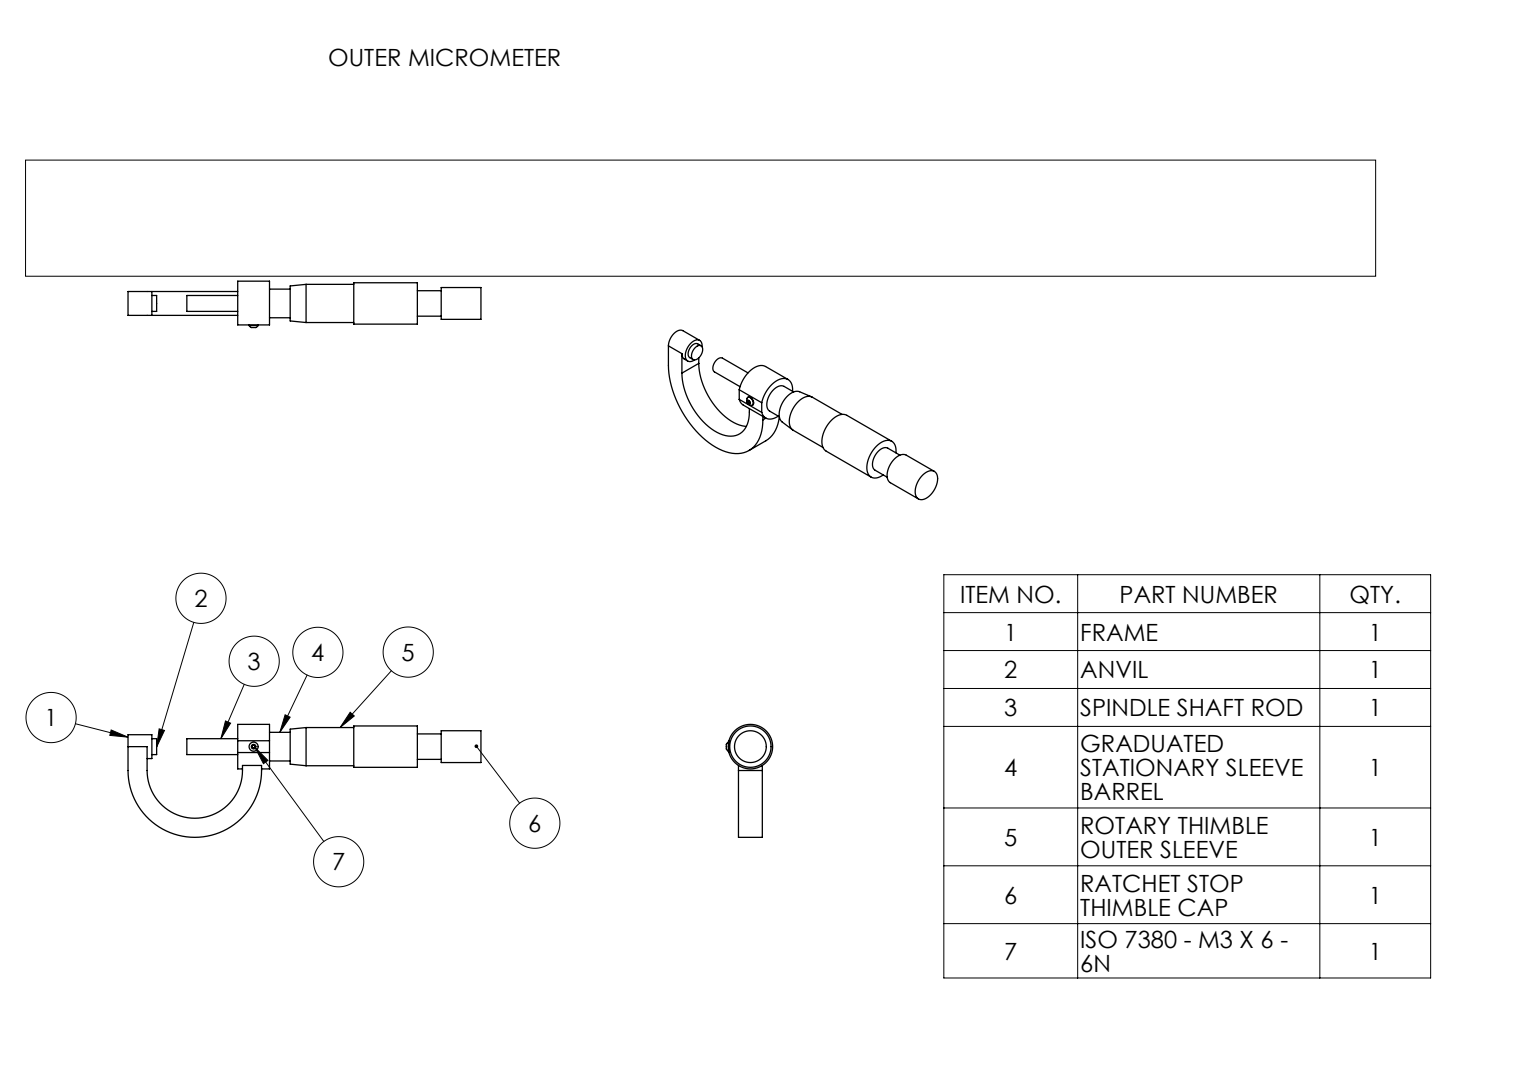
ISO-10303-21;
HEADER;
FILE_DESCRIPTION (('STEP AP214'),
    '1' );
FILE_NAME ('MAS-165',
    '2026-10-22T12:35:56',
    ( '' ),
    ( '' ),
    'SwSTEP 2.0',
    'SolidWorks 2026',
    '' );
FILE_SCHEMA (( 'AUTOMOTIVE_DESIGN' ));
ENDSEC;

DATA;
#1 = CARTESIAN_POINT ( 'NONE',  ( -30.00000000000000000, -8.316621552948000372E-15, 7.500000000000000000 ) ) ;
#2 = ORIENTED_EDGE ( 'NONE', *, *, #1476, .F. ) ;
#3 = EDGE_CURVE ( 'NONE', #403, #2721, #1745, .T. ) ;
#4 = DIRECTION ( 'NONE',  ( 0.000000000000000000, -1.000000000000000000, 0.000000000000000000 ) ) ;
#5 = FILL_AREA_STYLE_COLOUR ( '', #2827 ) ;
#6 = CYLINDRICAL_SURFACE ( 'NONE', #446, 5.000000000000000888 ) ;
#7 = EDGE_CURVE ( 'NONE', #417, #1789, #1947, .T. ) ;
#8 = PRODUCT_DEFINITION_SHAPE ( 'NONE', 'NONE',  #499 ) ;
#9 = PLANE ( 'NONE',  #1983 ) ;
#10 = VECTOR ( 'NONE', #970, 1000.000000000000000 ) ;
#11 = ORIENTED_EDGE ( 'NONE', *, *, #1483, .T. ) ;
#12 = VECTOR ( 'NONE', #2247, 1000.000000000000000 ) ;
#13 = ORIENTED_EDGE ( 'NONE', *, *, #713, .T. ) ;
#14 = VECTOR ( 'NONE', #2502, 1000.000000000000000 ) ;
#15 = CARTESIAN_POINT ( 'NONE',  ( 41.99999999999999289, -11.82159041753687845, 15.00000000000000000 ) ) ;
#16 = CARTESIAN_POINT ( 'NONE',  ( 37.48326775981565362, -1.423407605072588344, 16.38680797912482134 ) ) ;
#17 = DIRECTION ( 'NONE',  ( -0.000000000000000000, -0.000000000000000000, 1.000000000000000000 ) ) ;
#18 = STYLED_ITEM ( 'NONE', ( #223 ), #2456 ) ;
#19 = PRODUCT_DEFINITION_FORMATION_WITH_SPECIFIED_SOURCE ( 'ANY', '', #2257, .NOT_KNOWN. ) ;
#20 = LINE ( 'NONE', #2499, #1316 ) ;
#21 = PRESENTATION_STYLE_ASSIGNMENT (( #2824 ) ) ;
#22 = EDGE_LOOP ( 'NONE', ( #912, #3109, #1400, #258 ) ) ;
#23 = CARTESIAN_POINT ( 'NONE',  ( -26.99999999999999645, -7.622732162557277534E-15, 7.500000000000000000 ) ) ;
#24 = ADVANCED_FACE ( 'NONE', ( #42 ), #1841, .F. ) ;
#25 = DIRECTION ( 'NONE',  ( 0.000000000000000000, 0.000000000000000000, 1.000000000000000000 ) ) ;
#26 = CARTESIAN_POINT ( 'NONE',  ( 1.040000000000000036, 0.5773502691896263972, 1.000000000000000000 ) ) ;
#27 = MANIFOLD_SOLID_BREP ( 'Hex', #3139 ) ;
#28 = EDGE_CURVE ( 'NONE', #1232, #2394, #2025, .T. ) ;
#29 = ADVANCED_FACE ( 'NONE', ( #74 ), #315, .T. ) ;
#30 = ORIENTED_EDGE ( 'NONE', *, *, #3, .T. ) ;
#31 = CARTESIAN_POINT ( 'NONE',  ( 100.0000000000000000, -5.826660652933936785E-15, -1.499999999999999556 ) ) ;
#32 = CIRCLE ( 'NONE', #2124, 4.999999999999998224 ) ;
#33 = CARTESIAN_POINT ( 'NONE',  ( 30.00000000000000355, -15.00000000000000355, 15.00000000000000000 ) ) ;
#34 = DIRECTION ( 'NONE',  ( 1.000000000000000000, 2.312964634635742957E-16, 0.000000000000000000 ) ) ;
#35 = LINE ( 'NONE', #521, #2562 ) ;
#36 = CIRCLE ( 'NONE', #2432, 1.500000000000001332 ) ;
#37 = SHAPE_REPRESENTATION_RELATIONSHIP ( 'NONE' , 'NONE' ,  #2080, #2456 ) ;
#38 = EDGE_LOOP ( 'NONE', ( #1130, #2572 ) ) ;
#39 = DIRECTION ( 'NONE',  ( -0.000000000000000000, -0.000000000000000000, 1.000000000000000000 ) ) ;
#40 = DIRECTION ( 'NONE',  ( 0.000000000000000000, 0.000000000000000000, -1.000000000000000000 ) ) ;
#41 = CARTESIAN_POINT ( 'NONE',  ( 155.0000000000000284, -6.316519372592878167E-15, 2.499999999999999556 ) ) ;
#42 = FACE_OUTER_BOUND ( 'NONE', #272, .T. ) ;
#43 = ORIENTED_EDGE ( 'NONE', *, *, #1446, .F. ) ;
#44 = EDGE_CURVE ( 'NONE', #1232, #2037, #954, .T. ) ;
#45 = CIRCLE ( 'NONE', #370, 1.000000000000000000 ) ;
#46 = DIRECTION ( 'NONE',  ( 1.000000000000000000, 0.000000000000000000, 0.000000000000000000 ) ) ;
#47 = DIRECTION ( 'NONE',  ( 0.5150380749100542666, 1.049727191138618572E-16, 0.8571673007021122226 ) ) ;
#48 = DIRECTION ( 'NONE',  ( 0.000000000000000000, 1.000000000000000000, 0.000000000000000000 ) ) ;
#49 = ORIENTED_EDGE ( 'NONE', *, *, #85, .F. ) ;
#50 = SPHERICAL_SURFACE ( 'NONE', #2615, 3.351416843938785028 ) ;
#51 = EDGE_CURVE ( 'NONE', #357, #1877, #2331, .T. ) ;
#52 = ORIENTED_EDGE ( 'NONE', *, *, #1044, .F. ) ;
#53 = AXIS2_PLACEMENT_3D ( 'NONE', #2212, #1162, #2179 ) ;
#54 = CARTESIAN_POINT ( 'NONE',  ( 35.50000000000001421, 0.09798730130381244630, 16.49999999999999645 ) ) ;
#55 = DIRECTION ( 'NONE',  ( -0.000000000000000000, -0.000000000000000000, 1.000000000000000000 ) ) ;
#56 = VERTEX_POINT ( 'NONE', #623 ) ;
#57 = ORIENTED_EDGE ( 'NONE', *, *, #1286, .T. ) ;
#58 = VECTOR ( 'NONE', #2842, 1000.000000000000000 ) ;
#59 = DIRECTION ( 'NONE',  ( -1.000000000000000000, -0.000000000000000000, -0.000000000000000000 ) ) ;
#60 = DIRECTION ( 'NONE',  ( -2.478176394252581634E-16, 1.000000000000000000, 0.000000000000000000 ) ) ;
#61 = CLOSED_SHELL ( 'NONE', ( #1282, #587, #178, #1971, #3042, #967, #2402, #1991, #3073, #2520 ) ) ;
#62 = ADVANCED_FACE ( 'NONE', ( #2597 ), #606, .F. ) ;
#63 = COLOUR_RGB ( '',0.8941176470588234615, 0.8941176470588234615, 0.8941176470588234615 ) ;
#64 = ORIENTED_EDGE ( 'NONE', *, *, #1192, .F. ) ;
#65 = DIRECTION ( 'NONE',  ( 1.000000000000000000, 0.000000000000000000, 0.000000000000000000 ) ) ;
#66 = AXIS2_PLACEMENT_3D ( 'NONE', #1107, #1144, #2625 ) ;
#67 = CIRCLE ( 'NONE', #2220, 5.000000000000000000 ) ;
#68 = CARTESIAN_POINT ( 'NONE',  ( 180.0000000000000284, -6.928842772166554697E-15, 7.500000000000000000 ) ) ;
#69 = ORIENTED_EDGE ( 'NONE', *, *, #671, .F. ) ;
#70 = AXIS2_PLACEMENT_3D ( 'NONE', #1626, #2838, #1608 ) ;
#71 = CARTESIAN_POINT ( 'NONE',  ( 38.30162487582177278, 0.7519129166725618818, 16.46890859085320358 ) ) ;
#72 = DIRECTION ( 'NONE',  ( -0.000000000000000000, -0.000000000000000000, 1.000000000000000000 ) ) ;
#73 = CARTESIAN_POINT ( 'NONE',  ( 36.00776062886355078, -1.129166992945587866, 16.42915638304272363 ) ) ;
#74 = FACE_OUTER_BOUND ( 'NONE', #1738, .T. ) ;
#75 = ORIENTED_EDGE ( 'NONE', *, *, #1227, .F. ) ;
#76 = EDGE_CURVE ( 'NONE', #916, #1503, #2106, .T. ) ;
#77 = DIRECTION ( 'NONE',  ( 1.000000000000000000, 2.312964634635742957E-16, 0.000000000000000000 ) ) ;
#78 = CARTESIAN_POINT ( 'NONE',  ( 180.0000000000000284, -6.928842772166554697E-15, 7.500000000000000000 ) ) ;
#79 = VERTEX_POINT ( 'NONE', #2378 ) ;
#80 = DIRECTION ( 'NONE',  ( 1.000000000000000000, 0.000000000000000000, 0.000000000000000000 ) ) ;
#81 = AXIS2_PLACEMENT_3D ( 'NONE', #778, #1048, #1778 ) ;
#82 = CARTESIAN_POINT ( 'NONE',  ( 0.000000000000000000, -1.154700538379251684, -1.199226976249124676E-17 ) ) ;
#83 = ORIENTED_EDGE ( 'NONE', *, *, #909, .F. ) ;
#84 = AXIS2_PLACEMENT_3D ( 'NONE', #1775, #288, #1276 ) ;
#85 = EDGE_CURVE ( 'NONE', #373, #1694, #545, .T. ) ;
#86 = DIRECTION ( 'NONE',  ( -2.312964634635742957E-16, 1.000000000000000000, 0.000000000000000000 ) ) ;
#87 = VERTEX_POINT ( 'NONE', #874 ) ;
#88 = EDGE_LOOP ( 'NONE', ( #2505, #344, #500, #2889 ) ) ;
#89 = CARTESIAN_POINT ( 'NONE',  ( 70.00000000000032685, -6.928842772166554697E-15, 7.500000000000000000 ) ) ;
#90 = DIRECTION ( 'NONE',  ( -1.000000000000000000, -0.000000000000000000, -0.000000000000000000 ) ) ;
#91 = VERTEX_POINT ( 'NONE', #398 ) ;
#92 = CARTESIAN_POINT ( 'NONE',  ( 100.0000000000000000, -6.928842772166554697E-15, 7.500000000000000000 ) ) ;
#93 = CARTESIAN_POINT ( 'NONE',  ( 1.040000000000000036, 0.000000000000000000, 0.000000000000000000 ) ) ;
#94 = SHAPE_DEFINITION_REPRESENTATION ( #2508, #2591 ) ;
#95 = AXIS2_PLACEMENT_3D ( 'NONE', #1120, #2857, #636 ) ;
#96 = ORIENTED_EDGE ( 'NONE', *, *, #1476, .T. ) ;
#97 = ORIENTED_EDGE ( 'NONE', *, *, #671, .T. ) ;
#98 = DIRECTION ( 'NONE',  ( 0.000000000000000000, 0.000000000000000000, -1.000000000000000000 ) ) ;
#99 = CARTESIAN_POINT ( 'NONE',  ( 37.00000000000000000, 1.474514954580286030E-14, 20.99999999999999645 ) ) ;
#100 = ADVANCED_FACE ( 'NONE', ( #2884 ), #1598, .T. ) ;
#101 = EDGE_CURVE ( 'NONE', #738, #770, #2722, .T. ) ;
#102 = AXIS2_PLACEMENT_3D ( 'NONE', #2450, #1198, #3216 ) ;
#103 = PLANE ( 'NONE',  #1529 ) ;
#104 = EDGE_CURVE ( 'NONE', #415, #2077, #2930, .T. ) ;
#105 = ORIENTED_EDGE ( 'NONE', *, *, #2070, .F. ) ;
#106 = VERTEX_POINT ( 'NONE', #1616 ) ;
#107 = CARTESIAN_POINT ( 'NONE',  ( 38.45998082922275785, -0.3957415549423216605, 16.49311123862704775 ) ) ;
#108 = VERTEX_POINT ( 'NONE', #3091 ) ;
#109 =( REPRESENTATION_RELATIONSHIP ('NONE','NONE', #2426, #1116 ) REPRESENTATION_RELATIONSHIP_WITH_TRANSFORMATION ( #979 )SHAPE_REPRESENTATION_RELATIONSHIP( ) );
#110 = AXIS2_PLACEMENT_3D ( 'NONE', #2236, #2915, #685 ) ;
#111 = CARTESIAN_POINT ( 'NONE',  ( 0.000000000000000000, -0.5773502691896253980, -1.000000000000000000 ) ) ;
#112 = CLOSED_SHELL ( 'NONE', ( #233, #2010, #1720, #1045 ) ) ;
#113 = DIRECTION ( 'NONE',  ( 1.000000000000000000, 0.000000000000000000, 0.000000000000000000 ) ) ;
#114 = EDGE_LOOP ( 'NONE', ( #3092, #726, #1252, #1993 ) ) ;
#115 = CIRCLE ( 'NONE', #2264, 11.00000000000000355 ) ;
#116 = VECTOR ( 'NONE', #3173, 1000.000000000000000 ) ;
#117 = ORIENTED_EDGE ( 'NONE', *, *, #85, .T. ) ;
#118 = DIRECTION ( 'NONE',  ( 0.000000000000000000, 0.000000000000000000, -1.000000000000000000 ) ) ;
#119 = PRODUCT_DEFINITION_SHAPE ( 'NONE', 'NONE',  #694 ) ;
#120 = DIRECTION ( 'NONE',  ( 1.000000000000000000, 2.312964634635742957E-16, -0.000000000000000000 ) ) ;
#121 = AXIS2_PLACEMENT_3D ( 'NONE', #2014, #774, #60 ) ;
#122 = MECHANICAL_DESIGN_GEOMETRIC_PRESENTATION_REPRESENTATION (  '', ( #1113 ), #303 ) ;
#123 = ADVANCED_FACE ( 'NONE', ( #1123 ), #857, .F. ) ;
#124 = DIRECTION ( 'NONE',  ( 0.000000000000000000, 0.000000000000000000, 1.000000000000000000 ) ) ;
#125 = EDGE_LOOP ( 'NONE', ( #1383, #1724 ) ) ;
#126 = CARTESIAN_POINT ( 'NONE',  ( 38.49999999999999289, 1.474514954580286030E-14, 20.99999999999999645 ) ) ;
#127 = ADVANCED_FACE ( 'NONE', ( #378 ), #1155, .F. ) ;
#128 = ADVANCED_FACE ( 'NONE', ( #911 ), #1859, .T. ) ;
#129 = ORIENTED_EDGE ( 'NONE', *, *, #314, .F. ) ;
#130 = FACE_OUTER_BOUND ( 'NONE', #879, .T. ) ;
#131 = ORIENTED_EDGE ( 'NONE', *, *, #566, .F. ) ;
#132 = CARTESIAN_POINT ( 'NONE',  ( 155.0000000000000284, -5.949125332848671934E-15, -0.5000000000000004441 ) ) ;
#133 = APPLICATION_CONTEXT ( 'automotive_design' ) ;
#134 = CYLINDRICAL_SURFACE ( 'NONE', #2744, 14.00000000000000000 ) ;
#135 = DIRECTION ( 'NONE',  ( 0.000000000000000000, 0.000000000000000000, 1.000000000000000000 ) ) ;
#136 = ORIENTED_EDGE ( 'NONE', *, *, #525, .F. ) ;
#137 = VERTEX_POINT ( 'NONE', #2139 ) ;
#138 = DIRECTION ( 'NONE',  ( 0.000000000000000000, 0.000000000000000000, 1.000000000000000000 ) ) ;
#139 = DIRECTION ( 'NONE',  ( 0.000000000000000000, 0.000000000000000000, 1.000000000000000000 ) ) ;
#140 = CONICAL_SURFACE ( 'NONE', #2380, 1.250000000000001110, 1.029744258676654090 ) ;
#141 = DIRECTION ( 'NONE',  ( 0.000000000000000000, 0.5000000000000000000, -0.8660254037844385966 ) ) ;
#142 = ORIENTED_EDGE ( 'NONE', *, *, #1580, .F. ) ;
#143 = CARTESIAN_POINT ( 'NONE',  ( 38.49999999999997868, 0.1985404316418196702, 16.49999999999998224 ) ) ;
#144 = ORIENTED_EDGE ( 'NONE', *, *, #1772, .F. ) ;
#145 = CARTESIAN_POINT ( 'NONE',  ( 1.750000000000000000, 0.000000000000000000, 1.599999999999999645 ) ) ;
#146 = ORIENTED_EDGE ( 'NONE', *, *, #761, .F. ) ;
#147 = EDGE_CURVE ( 'NONE', #1882, #2430, #639, .T. ) ;
#148 = CYLINDRICAL_SURFACE ( 'NONE', #941, 7.500000000000000000 ) ;
#149 = PRODUCT_RELATED_PRODUCT_CATEGORY ( 'part', '', ( #2237 ) ) ;
#151 = EDGE_CURVE ( 'NONE', #2355, #2373, #2846, .T. ) ;
#150 = CARTESIAN_POINT ( 'NONE',  ( 140.0000000000000000, -6.928842772166554697E-15, 15.50000000000000000 ) ) ;
#152 = ORIENTED_EDGE ( 'NONE', *, *, #660, .F. ) ;
#153 = DIRECTION ( 'NONE',  ( -1.000000000000000000, -2.312964634635742957E-16, -0.000000000000000000 ) ) ;
#154 = CARTESIAN_POINT ( 'NONE',  ( 7.650000000000000355, 0.000000000000000000, 1.219500000000000028 ) ) ;
#155 = CIRCLE ( 'NONE', #2344, 1.219500000000000028 ) ;
#156 = SURFACE_STYLE_USAGE ( .BOTH. , #409 ) ;
#157 = CIRCLE ( 'NONE', #321, 1.000000000000000000 ) ;
#158 = CARTESIAN_POINT ( 'NONE',  ( 41.99999999999999289, 6.449497959004948951E-15, 15.00000000000000000 ) ) ;
#159 = ORIENTED_EDGE ( 'NONE', *, *, #497, .T. ) ;
#160 = DIRECTION ( 'NONE',  ( 0.000000000000000000, 0.000000000000000000, 1.000000000000000000 ) ) ;
#161 = AXIS2_PLACEMENT_3D ( 'NONE', #1164, #1184, #2943 ) ;
#162 = ORIENTED_EDGE ( 'NONE', *, *, #2964, .F. ) ;
#163 = VERTEX_POINT ( 'NONE', #411 ) ;
#164 = FACE_OUTER_BOUND ( 'NONE', #1049, .T. ) ;
#165 = ADVANCED_FACE ( 'NONE', ( #2345 ), #2393, .F. ) ;
#166 = CARTESIAN_POINT ( 'NONE',  ( 140.0000000000000000, -6.928842772166554697E-15, 7.500000000000000000 ) ) ;
#167 = DIRECTION ( 'NONE',  ( -0.000000000000000000, -0.000000000000000000, -1.000000000000000000 ) ) ;
#168 = PRODUCT_CONTEXT ( 'NONE', #3176, 'mechanical' ) ;
#169 = VERTEX_POINT ( 'NONE', #2407 ) ;
#170 = SURFACE_STYLE_USAGE ( .BOTH. , #3188 ) ;
#171 = FACE_OUTER_BOUND ( 'NONE', #213, .T. ) ;
#172 = AXIS2_PLACEMENT_3D ( 'NONE', #834, #880, #1605 ) ;
#173 = CIRCLE ( 'NONE', #1423, 12.00000000000000000 ) ;
#174 = CIRCLE ( 'NONE', #2003, 12.00000000000000000 ) ;
#175 = DIRECTION ( 'NONE',  ( 0.000000000000000000, -0.8660254037844387076, 0.5000000000000001110 ) ) ;
#176 = ADVANCED_FACE ( 'NONE', ( #427 ), #103, .T. ) ;
#177 = ORIENTED_EDGE ( 'NONE', *, *, #295, .F. ) ;
#178 = ADVANCED_FACE ( 'NONE', ( #1464 ), #509, .T. ) ;
#179 = DIRECTION ( 'NONE',  ( -2.312964634635742957E-16, 1.000000000000000000, 0.000000000000000000 ) ) ;
#180 = PRESENTATION_LAYER_ASSIGNMENT (  '', '', ( #18 ) ) ;
#181 = EDGE_LOOP ( 'NONE', ( #2444, #2735 ) ) ;
#182 = SURFACE_STYLE_FILL_AREA ( #1677 ) ;
#183 = ORIENTED_EDGE ( 'NONE', *, *, #207, .F. ) ;
#184 = EDGE_CURVE ( 'NONE', #3095, #2373, #706, .T. ) ;
#185 = DIRECTION ( 'NONE',  ( -0.000000000000000000, -0.000000000000000000, 1.000000000000000000 ) ) ;
#186 = CARTESIAN_POINT ( 'NONE',  ( 140.0000000000000000, -6.928842772166554697E-15, 12.50000000000000000 ) ) ;
#187 = CARTESIAN_POINT ( 'NONE',  ( -998.3826497308103853, 0.000000000000000000, 0.000000000000000000 ) ) ;
#188 = CONTEXT_DEPENDENT_SHAPE_REPRESENTATION ( #2861, #1874 ) ;
#189 =( LENGTH_UNIT ( ) NAMED_UNIT ( * ) SI_UNIT ( .MILLI., .METRE. ) );
#190 = DIRECTION ( 'NONE',  ( 1.000000000000000000, -0.000000000000000000, -0.000000000000000000 ) ) ;
#191 =( NAMED_UNIT ( * ) PLANE_ANGLE_UNIT ( ) SI_UNIT ( $, .RADIAN. ) );
#192 = EDGE_CURVE ( 'NONE', #1084, #211, #1163, .T. ) ;
#193 = CIRCLE ( 'NONE', #2951, 14.00000000000000000 ) ;
#194 = CARTESIAN_POINT ( 'NONE',  ( 155.0000000000000284, -6.928842772166554697E-15, 7.500000000000000000 ) ) ;
#195 = CIRCLE ( 'NONE', #1445, 10.00000000000000178 ) ;
#196 = CARTESIAN_POINT ( 'NONE',  ( 35.50000000000000000, 0.1959257125632855590, 16.50000000000000000 ) ) ;
#197 = ORIENTED_EDGE ( 'NONE', *, *, #540, .T. ) ;
#198 = CYLINDRICAL_SURFACE ( 'NONE', #340, 1.499999999999994449 ) ;
#199 = ORIENTED_EDGE ( 'NONE', *, *, #759, .F. ) ;
#200 = DIRECTION ( 'NONE',  ( 0.000000000000000000, 0.5000000000000003331, 0.8660254037844383745 ) ) ;
#201 = AXIS2_PLACEMENT_3D ( 'NONE', #1093, #2094, #1700 ) ;
#202 = DIRECTION ( 'NONE',  ( 1.000000000000000000, 0.000000000000000000, 0.000000000000000000 ) ) ;
#203 = DIRECTION ( 'NONE',  ( 0.000000000000000000, 1.224646799147353207E-16, -1.000000000000000000 ) ) ;
#204 = LINE ( 'NONE', #1443, #277 ) ;
#205 = SURFACE_STYLE_FILL_AREA ( #2455 ) ;
#206 = CONICAL_SURFACE ( 'NONE', #1038, 4.999999999999998224, 1.029744258676654312 ) ;
#207 = EDGE_CURVE ( 'NONE', #1415, #1866, #1103, .T. ) ;
#208 = DIRECTION ( 'NONE',  ( 0.000000000000000000, 0.000000000000000000, 1.000000000000000000 ) ) ;
#209 = DIRECTION ( 'NONE',  ( 1.000000000000000000, 0.000000000000000000, 0.000000000000000000 ) ) ;
#210 = ADVANCED_FACE ( 'NONE', ( #1707 ), #1221, .T. ) ;
#211 = VERTEX_POINT ( 'NONE', #3209 ) ;
#212 = CARTESIAN_POINT ( 'NONE',  ( 180.0000000000000284, -5.704195973019200848E-15, -2.500000000000002220 ) ) ;
#213 = EDGE_LOOP ( 'NONE', ( #2871, #2225, #753, #2533, #2320 ) ) ;
#214 = DIRECTION ( 'NONE',  ( -1.000000000000000000, -0.000000000000000000, -0.000000000000000000 ) ) ;
#215 = AXIS2_PLACEMENT_3D ( 'NONE', #2706, #2727, #977 ) ;
#216 = CARTESIAN_POINT ( 'NONE',  ( -41.99999999999999289, -6.449497959004950529E-15, 0.000000000000000000 ) ) ;
#217 = DIRECTION ( 'NONE',  ( 0.000000000000000000, 0.000000000000000000, -1.000000000000000000 ) ) ;
#218 = DIRECTION ( 'NONE',  ( 1.000000000000000000, 0.000000000000000000, 0.000000000000000000 ) ) ;
#219 = SURFACE_STYLE_FILL_AREA ( #3171 ) ;
#220 = EDGE_CURVE ( 'NONE', #2839, #2850, #1722, .T. ) ;
#221 = CYLINDRICAL_SURFACE ( 'NONE', #842, 2.849999999999999645 ) ;
#222 = PRODUCT_DEFINITION_SHAPE ( 'NONE', 'NONE',  #3226 ) ;
#223 = PRESENTATION_STYLE_ASSIGNMENT (( #983 ) ) ;
#224 = AXIS2_PLACEMENT_3D ( 'NONE', #361, #2327, #86 ) ;
#225 = PRESENTATION_LAYER_ASSIGNMENT (  '', '', ( #595 ) ) ;
#226 = AXIS2_PLACEMENT_3D ( 'NONE', #781, #362, #1550 ) ;
#227 = DIRECTION ( 'NONE',  ( -1.000000000000000000, -2.312964634635742957E-16, 0.000000000000000000 ) ) ;
#228 = DIRECTION ( 'NONE',  ( 1.000000000000000000, 0.000000000000000000, 0.000000000000000000 ) ) ;
#229 = AXIS2_PLACEMENT_3D ( 'NONE', #2936, #1181, #25 ) ;
#230 = CIRCLE ( 'NONE', #1844, 13.00000000000000178 ) ;
#231 = ORIENTED_EDGE ( 'NONE', *, *, #2924, .F. ) ;
#232 = EDGE_LOOP ( 'NONE', ( #1435, #2607, #784, #823 ) ) ;
#233 = ADVANCED_FACE ( 'NONE', ( #2687 ), #1203, .T. ) ;
#234 = EDGE_CURVE ( 'NONE', #516, #770, #260, .T. ) ;
#235 = CARTESIAN_POINT ( 'NONE',  ( 38.45202114561162432, -0.3888602178275583632, 16.49210820886665374 ) ) ;
#236 = CARTESIAN_POINT ( 'NONE',  ( 100.0000000000000000, -6.928842772166554697E-15, 19.50000000000000000 ) ) ;
#237 = CARTESIAN_POINT ( 'NONE',  ( 37.21237719682158485, -0.3527350612243344563, 12.48805154969246978 ) ) ;
#238 = LINE ( 'NONE', #2000, #1057 ) ;
#239 = CARTESIAN_POINT ( 'NONE',  ( 7.650000000000000355, 0.000000000000000000, 0.000000000000000000 ) ) ;
#240 =( NAMED_UNIT ( * ) PLANE_ANGLE_UNIT ( ) SI_UNIT ( $, .RADIAN. ) );
#241 = VERTEX_POINT ( 'NONE', #734 ) ;
#242 = CARTESIAN_POINT ( 'NONE',  ( -23.99999999999999645, 4.999999999999993783, 7.500000000000000888 ) ) ;
#243 = APPLICATION_CONTEXT ( 'automotive_design' ) ;
#244 = DIRECTION ( 'NONE',  ( 0.000000000000000000, 0.000000000000000000, 1.000000000000000000 ) ) ;
#245 = ORIENTED_EDGE ( 'NONE', *, *, #981, .F. ) ;
#246 = CIRCLE ( 'NONE', #2580, 14.00000000000000000 ) ;
#247 = ORIENTED_EDGE ( 'NONE', *, *, #3182, .F. ) ;
#248 = PRODUCT_DEFINITION_SHAPE ( 'NONE', 'NONE',  #1659 ) ;
#249 = DIRECTION ( 'NONE',  ( 0.000000000000000000, 0.000000000000000000, 1.000000000000000000 ) ) ;
#250 = DIRECTION ( 'NONE',  ( -1.000000000000000000, -0.000000000000000000, -0.000000000000000000 ) ) ;
#251 = DIRECTION ( 'NONE',  ( 0.000000000000000000, 0.000000000000000000, -1.000000000000000000 ) ) ;
#252 = EDGE_CURVE ( 'NONE', #466, #91, #1941, .T. ) ;
#253 = PRODUCT_CONTEXT ( 'NONE', #2801, 'mechanical' ) ;
#254 = PRODUCT_DEFINITION ( 'UNKNOWN', '', #1654, #571 ) ;
#255 = LINE ( 'NONE', #1808, #442 ) ;
#256 = CARTESIAN_POINT ( 'NONE',  ( -37.00000000000000000, -9.935696797193021379E-15, 7.500000000000000000 ) ) ;
#257 = EDGE_CURVE ( 'NONE', #3213, #626, #2525, .T. ) ;
#258 = ORIENTED_EDGE ( 'NONE', *, *, #2595, .F. ) ;
#259 = CARTESIAN_POINT ( 'NONE',  ( 27.00000000000000000, 6.704247063196759979E-15, 7.500000000000000000 ) ) ;
#260 = LINE ( 'NONE', #242, #2360 ) ;
#261 = LINE ( 'NONE', #26, #3174 ) ;
#262 = ORIENTED_EDGE ( 'NONE', *, *, #615, .T. ) ;
#263 = AXIS2_PLACEMENT_3D ( 'NONE', #1782, #798, #1552 ) ;
#264 = EDGE_LOOP ( 'NONE', ( #371, #711 ) ) ;
#265 = DIRECTION ( 'NONE',  ( 0.000000000000000000, 0.000000000000000000, 1.000000000000000000 ) ) ;
#266 = DIRECTION ( 'NONE',  ( -2.478176394252581634E-16, 1.000000000000000000, 0.000000000000000000 ) ) ;
#267 = CARTESIAN_POINT ( 'NONE',  ( 36.63069504892280293, -0.2100771151993728880, 12.49609970571322570 ) ) ;
#268 = AXIS2_PLACEMENT_3D ( 'NONE', #899, #2909, #681 ) ;
#269 = CYLINDRICAL_SURFACE ( 'NONE', #1531, 1.250000000000001110 ) ;
#270 = EDGE_CURVE ( 'NONE', #2818, #2355, #2189, .T. ) ;
#271 = DIRECTION ( 'NONE',  ( -1.000000000000000000, -0.000000000000000000, -0.000000000000000000 ) ) ;
#272 = EDGE_LOOP ( 'NONE', ( #2012, #2992, #144 ) ) ;
#273 = EDGE_CURVE ( 'NONE', #3128, #417, #1689, .T. ) ;
#274 = EDGE_CURVE ( 'NONE', #3069, #572, #2103, .T. ) ;
#275 = LINE ( 'NONE', #3009, #3087 ) ;
#276 = DIRECTION ( 'NONE',  ( 1.000000000000000000, 0.000000000000000000, 0.000000000000000000 ) ) ;
#277 = VECTOR ( 'NONE', #2201, 1000.000000000000000 ) ;
#278 = PRODUCT_DEFINITION_SHAPE ( 'NONE', 'NONE',  #3225 ) ;
#279 = CARTESIAN_POINT ( 'NONE',  ( -41.99999999999999289, -1.109217911451089172E-14, 0.000000000000000000 ) ) ;
#280 = AXIS2_PLACEMENT_3D ( 'NONE', #2473, #2667, #2948 ) ;
#281 = DIRECTION ( 'NONE',  ( 1.000000000000000000, 0.000000000000000000, -0.000000000000000000 ) ) ;
#282 = CIRCLE ( 'NONE', #2213, 4.999999999999999112 ) ;
#283 = ORIENTED_EDGE ( 'NONE', *, *, #1044, .T. ) ;
#284 = AXIS2_PLACEMENT_3D ( 'NONE', #1975, #461, #492 ) ;
#285 = VECTOR ( 'NONE', #856, 1000.000000000000000 ) ;
#286 = CARTESIAN_POINT ( 'NONE',  ( 140.0000000000000000, -6.316519372592878167E-15, 2.499999999999999556 ) ) ;
#287 = CARTESIAN_POINT ( 'NONE',  ( 38.19805860116020568, -0.9234461779904078460, 16.45357685834587613 ) ) ;
#288 = DIRECTION ( 'NONE',  ( 1.000000000000000000, 2.312964634635742957E-16, 0.000000000000000000 ) ) ;
#289 = LINE ( 'NONE', #2050, #12 ) ;
#290 = PRODUCT_DEFINITION_CONTEXT ( 'detailed design', #3029, 'design' ) ;
#291 = CARTESIAN_POINT ( 'NONE',  ( 1.040000000000000036, 0.8660254037844390407, 0.5000000000000002220 ) ) ;
#292 = FILL_AREA_STYLE_COLOUR ( '', #2366 ) ;
#293 = ORIENTED_EDGE ( 'NONE', *, *, #2633, .T. ) ;
#294 = DIRECTION ( 'NONE',  ( 1.000000000000000000, 0.000000000000000000, 0.000000000000000000 ) ) ;
#295 = EDGE_CURVE ( 'NONE', #1128, #2739, #2239, .T. ) ;
#296 = ADVANCED_FACE ( 'NONE', ( #1851 ), #6, .F. ) ;
#297 = PLANE ( 'NONE',  #1247 ) ;
#298 = EDGE_CURVE ( 'NONE', #3130, #2427, #2917, .T. ) ;
#299 = ORIENTED_EDGE ( 'NONE', *, *, #397, .F. ) ;
#300 = DIRECTION ( 'NONE',  ( 0.000000000000000000, 0.000000000000000000, -1.000000000000000000 ) ) ;
#301 = AXIS2_PLACEMENT_3D ( 'NONE', #323, #2823, #614 ) ;
#302 = FACE_OUTER_BOUND ( 'NONE', #2160, .T. ) ;
#303 =( GEOMETRIC_REPRESENTATION_CONTEXT ( 3 ) GLOBAL_UNCERTAINTY_ASSIGNED_CONTEXT ( ( #2916 ) ) GLOBAL_UNIT_ASSIGNED_CONTEXT ( ( #3088, #2138, #2843 ) ) REPRESENTATION_CONTEXT ( 'NONE', 'WORKASPACE' ) );
#304 = CARTESIAN_POINT ( 'NONE',  ( 180.0000000000000284, -6.928842772166554697E-15, 7.500000000000000000 ) ) ;
#305 = ORIENTED_EDGE ( 'NONE', *, *, #748, .T. ) ;
#306 = DIRECTION ( 'NONE',  ( -1.000000000000000000, -0.000000000000000000, -0.000000000000000000 ) ) ;
#307 = PRODUCT_DEFINITION_CONTEXT ( 'detailed design', #2566, 'design' ) ;
#308 = DIRECTION ( 'NONE',  ( -1.000000000000000000, -2.312964634635742957E-16, 0.000000000000000000 ) ) ;
#309 =( NAMED_UNIT ( * ) SI_UNIT ( $, .STERADIAN. ) SOLID_ANGLE_UNIT ( ) );
#310 = VERTEX_POINT ( 'NONE', #723 ) ;
#311 =( REPRESENTATION_RELATIONSHIP ('NONE','NONE', #2426, #524 ) REPRESENTATION_RELATIONSHIP_WITH_TRANSFORMATION ( #2435 )SHAPE_REPRESENTATION_RELATIONSHIP( ) );
#312 = CARTESIAN_POINT ( 'NONE',  ( 37.00000000000000000, 1.474514954580286030E-14, 20.99999999999999645 ) ) ;
#313 = FACE_OUTER_BOUND ( 'NONE', #2374, .T. ) ;
#314 = EDGE_CURVE ( 'NONE', #1882, #2739, #2737, .T. ) ;
#315 = SPHERICAL_SURFACE ( 'NONE', #1477, 3.351416843938785028 ) ;
#316 = ORIENTED_EDGE ( 'NONE', *, *, #1433, .F. ) ;
#317 = DIRECTION ( 'NONE',  ( -2.312964634635742957E-16, 1.000000000000000000, -0.000000000000000000 ) ) ;
#318 = DIRECTION ( 'NONE',  ( -1.000000000000000000, -0.000000000000000000, -0.000000000000000000 ) ) ;
#319 = CARTESIAN_POINT ( 'NONE',  ( 100.0000000000000000, -5.826660652933936785E-15, -1.499999999999999556 ) ) ;
#320 = ORIENTED_EDGE ( 'NONE', *, *, #1335, .T. ) ;
#321 = AXIS2_PLACEMENT_3D ( 'NONE', #2470, #438, #717 ) ;
#322 = DIRECTION ( 'NONE',  ( 0.000000000000000000, 0.000000000000000000, -1.000000000000000000 ) ) ;
#323 = CARTESIAN_POINT ( 'NONE',  ( 87.00000000000000000, -7.622732162557277534E-15, 7.500000000000000000 ) ) ;
#324 = ORIENTED_EDGE ( 'NONE', *, *, #2185, .F. ) ;
#325 = ADVANCED_FACE ( 'NONE', ( #447 ), #1432, .F. ) ;
#326 = VECTOR ( 'NONE', #1980, 1000.000000000000000 ) ;
#327 = CARTESIAN_POINT ( 'NONE',  ( 38.49999999999999289, 1.474514954580286030E-14, 16.49999999999999289 ) ) ;
#328 = CARTESIAN_POINT ( 'NONE',  ( 1.649999999999999911, 1.959434878635764737E-16, -1.599999999999999645 ) ) ;
#329 = EDGE_CURVE ( 'NONE', #2636, #2004, #2214, .T. ) ;
#330 = SHAPE_REPRESENTATION ( 'Spindle Shaft Rod', ( #2878 ), #1321 ) ;
#331 = CARTESIAN_POINT ( 'NONE',  ( 27.00000000000000000, -7.622732162557277534E-15, 7.500000000000000000 ) ) ;
#332 = ORIENTED_EDGE ( 'NONE', *, *, #28, .F. ) ;
#333 = CIRCLE ( 'NONE', #2770, 14.00000000000000000 ) ;
#334 = CARTESIAN_POINT ( 'NONE',  ( 1.040000000000000036, 0.5773502691896263972, 1.000000000000000000 ) ) ;
#335 = CARTESIAN_POINT ( 'NONE',  ( -30.00000000000000000, -3.673940397442059178E-15, 0.000000000000000000 ) ) ;
#336 = ORIENTED_EDGE ( 'NONE', *, *, #257, .F. ) ;
#337 = EDGE_CURVE ( 'NONE', #658, #1756, #1956, .T. ) ;
#338 = FACE_OUTER_BOUND ( 'NONE', #1623, .T. ) ;
#339 = AXIS2_PLACEMENT_3D ( 'NONE', #2130, #2093, #2543 ) ;
#340 = AXIS2_PLACEMENT_3D ( 'NONE', #664, #915, #276 ) ;
#341 = AXIS2_PLACEMENT_3D ( 'NONE', #259, #1766, #1051 ) ;
#342 = DIRECTION ( 'NONE',  ( -1.000000000000000000, -0.000000000000000000, -0.000000000000000000 ) ) ;
#343 = PRESENTATION_STYLE_ASSIGNMENT (( #1574 ) ) ;
#344 = ORIENTED_EDGE ( 'NONE', *, *, #354, .T. ) ;
#345 = DIRECTION ( 'NONE',  ( 1.000000000000000000, 0.000000000000000000, 0.000000000000000000 ) ) ;
#346 = CYLINDRICAL_SURFACE ( 'NONE', #226, 14.00000000000000000 ) ;
#347 = CARTESIAN_POINT ( 'NONE',  ( 180.0000000000000284, -6.928842772166554697E-15, 17.50000000000000000 ) ) ;
#348 =( LENGTH_UNIT ( ) NAMED_UNIT ( * ) SI_UNIT ( .MILLI., .METRE. ) );
#349 = ORIENTED_EDGE ( 'NONE', *, *, #2340, .F. ) ;
#350 = CARTESIAN_POINT ( 'NONE',  ( 1.040000000000000036, -0.5773502691896253980, -1.000000000000000000 ) ) ;
#351 = DIRECTION ( 'NONE',  ( -0.000000000000000000, -0.5000000000000003331, -0.8660254037844383745 ) ) ;
#352 = EDGE_LOOP ( 'NONE', ( #52, #897, #2546 ) ) ;
#353 = FACE_OUTER_BOUND ( 'NONE', #1646, .T. ) ;
#354 = EDGE_CURVE ( 'NONE', #2839, #488, #2984, .T. ) ;
#355 = FACE_OUTER_BOUND ( 'NONE', #984, .T. ) ;
#356 = DIRECTION ( 'NONE',  ( 1.000000000000000000, 0.000000000000000000, 0.000000000000000000 ) ) ;
#357 = VERTEX_POINT ( 'NONE', #15 ) ;
#358 = AXIS2_PLACEMENT_3D ( 'NONE', #894, #2425, #1157 ) ;
#359 = VERTEX_POINT ( 'NONE', #740 ) ;
#360 = ADVANCED_FACE ( 'NONE', ( #1740 ), #714, .F. ) ;
#361 = CARTESIAN_POINT ( 'NONE',  ( 47.00000000000000000, 1.133017633246824530E-14, 7.500000000000000000 ) ) ;
#362 = DIRECTION ( 'NONE',  ( 1.000000000000000000, 2.312964634635742957E-16, 0.000000000000000000 ) ) ;
#363 = DIRECTION ( 'NONE',  ( -0.000000000000000000, -0.000000000000000000, -1.000000000000000000 ) ) ;
#364 = ORIENTED_EDGE ( 'NONE', *, *, #2262, .F. ) ;
#365 = CARTESIAN_POINT ( 'NONE',  ( 35.65194399346783882, -0.6651260505907211629, 16.47584948644689007 ) ) ;
#366 = CARTESIAN_POINT ( 'NONE',  ( 38.50000000000000000, -0.1985404316418107051, 16.49999999999999645 ) ) ;
#367 = ORIENTED_EDGE ( 'NONE', *, *, #1335, .F. ) ;
#368 = CARTESIAN_POINT ( 'NONE',  ( 140.0000000000000000, -6.928842772166554697E-15, 7.500000000000000000 ) ) ;
#369 = DIRECTION ( 'NONE',  ( -0.000000000000000000, 1.000000000000000000, 1.224646799147353207E-16 ) ) ;
#370 = AXIS2_PLACEMENT_3D ( 'NONE', #3118, #1653, #1136 ) ;
#371 = ORIENTED_EDGE ( 'NONE', *, *, #1189, .F. ) ;
#372 = EDGE_CURVE ( 'NONE', #87, #2397, #1009, .T. ) ;
#373 = VERTEX_POINT ( 'NONE', #2492 ) ;
#374 = CARTESIAN_POINT ( 'NONE',  ( -23.99999999999999645, -6.928842772166554697E-15, 7.500000000000000000 ) ) ;
#375 = DIRECTION ( 'NONE',  ( -0.000000000000000000, -0.000000000000000000, 1.000000000000000000 ) ) ;
#376 = ADVANCED_FACE ( 'NONE', ( #502 ), #991, .T. ) ;
#377 = AXIS2_PLACEMENT_3D ( 'NONE', #2479, #250, #1805 ) ;
#378 = FACE_OUTER_BOUND ( 'NONE', #1451, .T. ) ;
#379 = ORIENTED_EDGE ( 'NONE', *, *, #1424, .F. ) ;
#380 = UNCERTAINTY_MEASURE_WITH_UNIT (LENGTH_MEASURE( 1.000000000000000082E-05 ), #1214, 'distance_accuracy_value', 'NONE');
#381 = FACE_BOUND ( 'NONE', #577, .T. ) ;
#382 = ORIENTED_EDGE ( 'NONE', *, *, #1088, .F. ) ;
#383 = FACE_OUTER_BOUND ( 'NONE', #1369, .T. ) ;
#384 = ORIENTED_EDGE ( 'NONE', *, *, #1446, .T. ) ;
#385 = CARTESIAN_POINT ( 'NONE',  ( 1.040000000000000036, 0.000000000000000000, 0.000000000000000000 ) ) ;
#386 = AXIS2_PLACEMENT_3D ( 'NONE', #1799, #2316, #40 ) ;
#387 = FACE_OUTER_BOUND ( 'NONE', #22, .T. ) ;
#388 = DIRECTION ( 'NONE',  ( 1.000000000000000000, 0.000000000000000000, 0.000000000000000000 ) ) ;
#389 = EDGE_LOOP ( 'NONE', ( #1124, #807, #247, #64 ) ) ;
#390 = AXIS2_PLACEMENT_3D ( 'NONE', #3020, #1047, #980 ) ;
#391 = VERTEX_POINT ( 'NONE', #2955 ) ;
#392 = VECTOR ( 'NONE', #317, 1000.000000000000000 ) ;
#393 = DIRECTION ( 'NONE',  ( -1.000000000000000000, -2.312964634635742957E-16, 0.000000000000000000 ) ) ;
#394 = DIRECTION ( 'NONE',  ( -0.000000000000000000, 0.5000000000000003331, -0.8660254037844383745 ) ) ;
#395 = AXIS2_PLACEMENT_3D ( 'NONE', #2044, #2788, #565 ) ;
#396 = MECHANICAL_DESIGN_GEOMETRIC_PRESENTATION_REPRESENTATION (  '', ( #2111 ), #1957 ) ;
#397 = EDGE_CURVE ( 'NONE', #1789, #2998, #1521, .T. ) ;
#398 = CARTESIAN_POINT ( 'NONE',  ( 155.0000000000000284, -6.928842772166554697E-15, 17.50000000000000000 ) ) ;
#399 = ORIENTED_EDGE ( 'NONE', *, *, #2047, .T. ) ;
#400 = DIRECTION ( 'NONE',  ( -1.000000000000000000, -0.000000000000000000, -0.000000000000000000 ) ) ;
#401 = VERTEX_POINT ( 'NONE', #1491 ) ;
#402 = CARTESIAN_POINT ( 'NONE',  ( 100.0000000000000000, -6.928842772166554697E-15, 20.50000000000000000 ) ) ;
#403 = VERTEX_POINT ( 'NONE', #1979 ) ;
#404 = CARTESIAN_POINT ( 'NONE',  ( 0.000000000000000000, 3.490243377569956061E-16, -2.849999999999999645 ) ) ;
#405 = CYLINDRICAL_SURFACE ( 'NONE', #2026, 12.00000000000000000 ) ;
#406 = ORIENTED_EDGE ( 'NONE', *, *, #733, .T. ) ;
#407 = DIRECTION ( 'NONE',  ( 0.000000000000000000, 0.000000000000000000, -1.000000000000000000 ) ) ;
#408 = DIRECTION ( 'NONE',  ( 1.000000000000000000, 0.000000000000000000, 0.000000000000000000 ) ) ;
#409 = SURFACE_SIDE_STYLE ('',( #2405 ) ) ;
#410 = VECTOR ( 'NONE', #420, 1000.000000000000000 ) ;
#411 = CARTESIAN_POINT ( 'NONE',  ( 27.00000000000000000, 1.243235845170086479E-14, 16.49999999999999289 ) ) ;
#412 = ORIENTED_EDGE ( 'NONE', *, *, #843, .T. ) ;
#413 = CARTESIAN_POINT ( 'NONE',  ( 100.0000000000000000, -6.928842772166554697E-15, 7.500000000000000000 ) ) ;
#414 = ADVANCED_FACE ( 'NONE', ( #2258 ), #2743, .F. ) ;
#415 = VERTEX_POINT ( 'NONE', #482 ) ;
#416 = CARTESIAN_POINT ( 'NONE',  ( 35.50000000000000000, -7.622732095468789599E-15, 16.49999999999999289 ) ) ;
#417 = VERTEX_POINT ( 'NONE', #1239 ) ;
#418 = PLANE ( 'NONE',  #2778 ) ;
#419 = UNCERTAINTY_MEASURE_WITH_UNIT (LENGTH_MEASURE( 1.000000000000000082E-05 ), #2203, 'distance_accuracy_value', 'NONE');
#420 = DIRECTION ( 'NONE',  ( 1.000000000000000000, 2.312964634635742957E-16, 0.000000000000000000 ) ) ;
#421 = ORIENTED_EDGE ( 'NONE', *, *, #1100, .F. ) ;
#422 = CARTESIAN_POINT ( 'NONE',  ( 38.49999999999999289, -7.622732162557277534E-15, 16.49999999999999289 ) ) ;
#423 = DIRECTION ( 'NONE',  ( -3.854941057726241055E-16, 1.000000000000000000, 0.000000000000000000 ) ) ;
#424 = VECTOR ( 'NONE', #2474, 1000.000000000000000 ) ;
#425 =( LENGTH_UNIT ( ) NAMED_UNIT ( * ) SI_UNIT ( .MILLI., .METRE. ) );
#426 = PRESENTATION_LAYER_ASSIGNMENT (  '', '', ( #2250 ) ) ;
#427 = FACE_OUTER_BOUND ( 'NONE', #2786, .T. ) ;
#428 = EDGE_LOOP ( 'NONE', ( #2332, #810, #725 ) ) ;
#429 = CARTESIAN_POINT ( 'NONE',  ( 37.09819064725438409, 1.500059831078516703, 16.37410956135321882 ) ) ;
#430 = ORIENTED_EDGE ( 'NONE', *, *, #981, .T. ) ;
#431 = FACE_OUTER_BOUND ( 'NONE', #2490, .T. ) ;
#432 = ORIENTED_EDGE ( 'NONE', *, *, #882, .F. ) ;
#433 = DIRECTION ( 'NONE',  ( 1.000000000000000000, 0.000000000000000000, 0.000000000000000000 ) ) ;
#434 = DIRECTION ( 'NONE',  ( -2.312964634635742957E-16, 1.000000000000000000, 0.000000000000000000 ) ) ;
#435 = DIRECTION ( 'NONE',  ( 1.000000000000000000, 2.312964634635742957E-16, 0.000000000000000000 ) ) ;
#436 = EDGE_CURVE ( 'NONE', #1803, #211, #2967, .T. ) ;
#437 = PRODUCT_CONTEXT ( 'NONE', #1344, 'mechanical' ) ;
#438 = DIRECTION ( 'NONE',  ( -1.000000000000000000, -0.000000000000000000, -0.000000000000000000 ) ) ;
#439 = VECTOR ( 'NONE', #888, 1000.000000000000227 ) ;
#440 = CARTESIAN_POINT ( 'NONE',  ( -41.99999999999999289, -15.00000000000000711, 15.00000000000000000 ) ) ;
#441 =( NAMED_UNIT ( * ) SI_UNIT ( $, .STERADIAN. ) SOLID_ANGLE_UNIT ( ) );
#442 = VECTOR ( 'NONE', #760, 1000.000000000000000 ) ;
#443 = CLOSED_SHELL ( 'NONE', ( #3157, #127, #2028, #1449, #2628, #1324, #3219, #537, #1757, #1948, #128, #2460, #2730, #325, #210, #2684, #2552, #1070, #2797, #829, #2086, #2736, #3198, #1675, #3211 ) ) ;
#444 = UNCERTAINTY_MEASURE_WITH_UNIT (LENGTH_MEASURE( 1.000000000000000082E-05 ), #3138, 'distance_accuracy_value', 'NONE');
#445 = AXIS2_PLACEMENT_3D ( 'NONE', #594, #3096, #3064 ) ;
#446 = AXIS2_PLACEMENT_3D ( 'NONE', #986, #1989, #749 ) ;
#447 = FACE_OUTER_BOUND ( 'NONE', #1253, .T. ) ;
#448 = CARTESIAN_POINT ( 'NONE',  ( 38.19805860116023410, 0.9234461779904211687, 16.45357685834586903 ) ) ;
#449 = EDGE_LOOP ( 'NONE', ( #2891, #1302, #2981, #2325 ) ) ;
#450 = CYLINDRICAL_SURFACE ( 'NONE', #386, 8.999999999999994671 ) ;
#451 = ORIENTED_EDGE ( 'NONE', *, *, #3048, .T. ) ;
#452 = CARTESIAN_POINT ( 'NONE',  ( -26.99999999999999645, -7.622732162557277534E-15, 7.500000000000000000 ) ) ;
#453 = CARTESIAN_POINT ( 'NONE',  ( 1.649999999999999911, 3.490243377569956061E-16, -2.849999999999999645 ) ) ;
#454 = DIRECTION ( 'NONE',  ( 0.000000000000000000, 0.000000000000000000, 1.000000000000000000 ) ) ;
#455 = FILL_AREA_STYLE_COLOUR ( '', #987 ) ;
#456 = EDGE_CURVE ( 'NONE', #1944, #79, #2985, .T. ) ;
#457 = DIRECTION ( 'NONE',  ( 0.000000000000000000, 0.000000000000000000, -1.000000000000000000 ) ) ;
#458 =( NAMED_UNIT ( * ) SI_UNIT ( $, .STERADIAN. ) SOLID_ANGLE_UNIT ( ) );
#459 =( REPRESENTATION_RELATIONSHIP ('NONE','NONE', #2426, #2080 ) REPRESENTATION_RELATIONSHIP_WITH_TRANSFORMATION ( #2729 )SHAPE_REPRESENTATION_RELATIONSHIP( ) );
#460 = VECTOR ( 'NONE', #601, 999.9999999999998863 ) ;
#461 = DIRECTION ( 'NONE',  ( -1.000000000000000000, -2.312964634635742957E-16, -0.000000000000000000 ) ) ;
#462 = AXIS2_PLACEMENT_3D ( 'NONE', #2599, #1915, #160 ) ;
#463 = DIRECTION ( 'NONE',  ( -0.000000000000000000, -0.000000000000000000, 1.000000000000000000 ) ) ;
#464 = ORIENTED_EDGE ( 'NONE', *, *, #1403, .T. ) ;
#465 = EDGE_CURVE ( 'NONE', #572, #3069, #67, .T. ) ;
#466 = VERTEX_POINT ( 'NONE', #347 ) ;
#467 = LINE ( 'NONE', #3149, #2202 ) ;
#468 = CARTESIAN_POINT ( 'NONE',  ( 38.12949724085409287, -0.9918543271721246279, 16.44544909559323287 ) ) ;
#469 = DIRECTION ( 'NONE',  ( -0.000000000000000000, -0.000000000000000000, -1.000000000000000000 ) ) ;
#470 = DIRECTION ( 'NONE',  ( 0.000000000000000000, 0.000000000000000000, -1.000000000000000000 ) ) ;
#471 = SURFACE_STYLE_FILL_AREA ( #953 ) ;
#472 = CARTESIAN_POINT ( 'NONE',  ( -5.000000000000000000, -6.316519372592878167E-15, 12.50000000000000000 ) ) ;
#473 = AXIS2_PLACEMENT_3D ( 'NONE', #1752, #228, #2224 ) ;
#474 = CARTESIAN_POINT ( 'NONE',  ( 1.040000000000000036, 0.5773502691896263972, -1.000000000000000000 ) ) ;
#475 = ADVANCED_FACE ( 'NONE', ( #1758, #2466 ), #1952, .F. ) ;
#476 = TOROIDAL_SURFACE ( 'NONE', #2813, 1.599999999999999645, 0.1000000000000000056 ) ;
#477 = LINE ( 'NONE', #1223, #1086 ) ;
#478 = EDGE_LOOP ( 'NONE', ( #2640, #2192 ) ) ;
#479 = VERTEX_POINT ( 'NONE', #286 ) ;
#480 = FACE_OUTER_BOUND ( 'NONE', #886, .T. ) ;
#481 = B_SPLINE_CURVE_WITH_KNOTS ( 'NONE', 3,
 ( #609, #3129, #1643, #1588, #2584, #1338, #1883, #2554, #896, #1864 ),
 .UNSPECIFIED., .F., .F.,
 ( 4, 2, 2, 2, 4 ),
 ( 0.0002158803543021033892, 0.0005338002860526318500, 0.0008517202178031603108, 0.001169640149553688880, 0.001487560081304217232 ),
 .UNSPECIFIED. ) ;
#482 = CARTESIAN_POINT ( 'NONE',  ( 60.00000000000000000, -6.928842772166554697E-15, 16.50000000000000000 ) ) ;
#483 = FACE_OUTER_BOUND ( 'NONE', #2112, .T. ) ;
#484 = DIRECTION ( 'NONE',  ( 1.000000000000000000, 0.000000000000000000, 0.000000000000000000 ) ) ;
#485 = PRODUCT_CONTEXT ( 'NONE', #2078, 'mechanical' ) ;
#486 = DIRECTION ( 'NONE',  ( -1.000000000000000000, 0.000000000000000000, -0.000000000000000000 ) ) ;
#487 = SHAPE_REPRESENTATION_RELATIONSHIP ( 'NONE' , 'NONE' ,  #330, #3045 ) ;
#488 = VERTEX_POINT ( 'NONE', #1274 ) ;
#489=STYLED_ITEM('',(#3271),#1054);
#490 = AXIS2_PLACEMENT_3D ( 'NONE', #3159, #891, #141 ) ;
#491 =( GEOMETRIC_REPRESENTATION_CONTEXT ( 3 ) GLOBAL_UNCERTAINTY_ASSIGNED_CONTEXT ( ( #2017 ) ) GLOBAL_UNIT_ASSIGNED_CONTEXT ( ( #605, #1315, #1563 ) ) REPRESENTATION_CONTEXT ( 'NONE', 'WORKASPACE' ) );
#492 = DIRECTION ( 'NONE',  ( 0.000000000000000000, -1.000000000000000000, 0.000000000000000000 ) ) ;
#493 = CIRCLE ( 'NONE', #3140, 12.00000000000000000 ) ;
#494 = FACE_OUTER_BOUND ( 'NONE', #181, .T. ) ;
#495 = CIRCLE ( 'NONE', #1644, 13.00000000000000178 ) ;
#496 = AXIS2_PLACEMENT_3D ( 'NONE', #1455, #2509, #249 ) ;
#497 = EDGE_CURVE ( 'NONE', #2088, #3100, #2946, .T. ) ;
#498 = ORIENTED_EDGE ( 'NONE', *, *, #1931, .T. ) ;
#499 = PRODUCT_DEFINITION ( 'UNKNOWN', '', #758, #2762 ) ;
#500 = ORIENTED_EDGE ( 'NONE', *, *, #591, .T. ) ;
#501 = MECHANICAL_DESIGN_GEOMETRIC_PRESENTATION_REPRESENTATION (  '', ( #18 ), #1537 ) ;
#502 = FACE_OUTER_BOUND ( 'NONE', #3012, .T. ) ;
#503 = CARTESIAN_POINT ( 'NONE',  ( 7.650000000000000355, 0.000000000000000000, 0.000000000000000000 ) ) ;
#504 = PLANE ( 'NONE',  #2021 ) ;
#505 = FACE_BOUND ( 'NONE', #645, .T. ) ;
#506 =( NAMED_UNIT ( * ) SI_UNIT ( $, .STERADIAN. ) SOLID_ANGLE_UNIT ( ) );
#507 = EDGE_LOOP ( 'NONE', ( #1692, #1273, #197, #3052 ) ) ;
#508 = CARTESIAN_POINT ( 'NONE',  ( 35.50982285435565444, 0.1975270956567308500, 16.49834805537327043 ) ) ;
#509 = CYLINDRICAL_SURFACE ( 'NONE', #747, 8.000000000000000000 ) ;
#510 = EDGE_CURVE ( 'NONE', #211, #1084, #174, .T. ) ;
#511 = DIRECTION ( 'NONE',  ( 1.000000000000000000, 0.000000000000000000, 0.000000000000000000 ) ) ;
#512 = CIRCLE ( 'NONE', #301, 8.999999999999992895 ) ;
#513 = ORIENTED_EDGE ( 'NONE', *, *, #2779, .F. ) ;
#514 = SHAPE_REPRESENTATION ( 'frame', ( #2878 ), #491 ) ;
#515 = CIRCLE ( 'NONE', #769, 14.00000000000000000 ) ;
#516 = VERTEX_POINT ( 'NONE', #608 ) ;
#517 = EDGE_CURVE ( 'NONE', #3213, #1108, #2029, .T. ) ;
#518 = CARTESIAN_POINT ( 'NONE',  ( 38.34772064623945198, -0.6658172387807467230, 16.47579882838004295 ) ) ;
#519 = DIRECTION ( 'NONE',  ( -0.000000000000000000, 0.5000000000000000000, 0.8660254037844385966 ) ) ;
#520 = CARTESIAN_POINT ( 'NONE',  ( 1.269999999999999796, 0.000000000000000000, 0.000000000000000000 ) ) ;
#521 = CARTESIAN_POINT ( 'NONE',  ( 1.040000000000000036, 1.154700538379252350, -1.084202172485497162E-16 ) ) ;
#522 = DIRECTION ( 'NONE',  ( -0.000000000000000000, -0.000000000000000000, 1.000000000000000000 ) ) ;
#523 = ORIENTED_EDGE ( 'NONE', *, *, #2382, .F. ) ;
#524 = SHAPE_REPRESENTATION ( 'socket button head screw_iso_ISO 7380 - M3 x 6 - 6N', ( #2878 ), #1010 ) ;
#525 = EDGE_CURVE ( 'NONE', #974, #2998, #2583, .T. ) ;
#526 = CARTESIAN_POINT ( 'NONE',  ( 37.92226537325436198, 1.198992358192679797, 16.42086068928975706 ) ) ;
#527 = SURFACE_STYLE_USAGE ( .BOTH. , #2428 ) ;
#528 = CARTESIAN_POINT ( 'NONE',  ( 100.0000000000000000, -5.459266613189731341E-15, -4.500000000000000888 ) ) ;
#529 = ORIENTED_EDGE ( 'NONE', *, *, #1753, .F. ) ;
#530 = CIRCLE ( 'NONE', #1202, 8.999999999999989342 ) ;
#531 = VERTEX_POINT ( 'NONE', #845 ) ;
#532 = DIRECTION ( 'NONE',  ( 1.000000000000000000, 2.312964634635742957E-16, 0.000000000000000000 ) ) ;
#533 = CARTESIAN_POINT ( 'NONE',  ( 37.99089481476345753, -1.130332597043731901, 16.42900728359812135 ) ) ;
#534 = PLANE ( 'NONE',  #3005 ) ;
#535 = VECTOR ( 'NONE', #185, 1000.000000000000000 ) ;
#536 = CYLINDRICAL_SURFACE ( 'NONE', #1581, 13.00000000000000178 ) ;
#537 = ADVANCED_FACE ( 'NONE', ( #579 ), #1568, .T. ) ;
#538 = CARTESIAN_POINT ( 'NONE',  ( -26.99999999999999645, -7.622732162557277534E-15, 7.500000000000000000 ) ) ;
#539 = ORIENTED_EDGE ( 'NONE', *, *, #274, .T. ) ;
#540 = EDGE_CURVE ( 'NONE', #2776, #241, #816, .T. ) ;
#541 = LINE ( 'NONE', #1281, #285 ) ;
#542 = SURFACE_STYLE_FILL_AREA ( #2023 ) ;
#543 = CIRCLE ( 'NONE', #2666, 9.000000000000000000 ) ;
#544 = CYLINDRICAL_SURFACE ( 'NONE', #1147, 5.000000000000000888 ) ;
#545 = CIRCLE ( 'NONE', #2775, 3.351416843938785028 ) ;
#546 = VERTEX_POINT ( 'NONE', #31 ) ;
#547 = CIRCLE ( 'NONE', #2359, 2.849999999999999645 ) ;
#548 = VERTEX_POINT ( 'NONE', #831 ) ;
#549 = VECTOR ( 'NONE', #1448, 1000.000000000000000 ) ;
#550 = CIRCLE ( 'NONE', #2314, 1.000000000000000000 ) ;
#551 = AXIS2_PLACEMENT_3D ( 'NONE', #3000, #773, #2215 ) ;
#552 = CARTESIAN_POINT ( 'NONE',  ( 35.80758137781342043, -0.9152444266664223615, 16.45371270176149991 ) ) ;
#553 = CARTESIAN_POINT ( 'NONE',  ( 35.68903409116789760, -0.7546922429561464529, 16.47012649564899078 ) ) ;
#554 = DIRECTION ( 'NONE',  ( -1.000000000000000000, -0.000000000000000000, -0.000000000000000000 ) ) ;
#555 = ORIENTED_EDGE ( 'NONE', *, *, #1912, .F. ) ;
#556 = CARTESIAN_POINT ( 'NONE',  ( 70.00000000000032685, -6.928842772166554697E-15, 19.50000000000000000 ) ) ;
#557 =( LENGTH_UNIT ( ) NAMED_UNIT ( * ) SI_UNIT ( .MILLI., .METRE. ) );
#558 = ORIENTED_EDGE ( 'NONE', *, *, #735, .T. ) ;
#559 = EDGE_CURVE ( 'NONE', #3128, #1393, #1428, .T. ) ;
#560 = PRODUCT_RELATED_PRODUCT_CATEGORY ( 'part', '', ( #2257 ) ) ;
#561 = CARTESIAN_POINT ( 'NONE',  ( 35.50000000000000000, 1.243235838461289750E-14, 16.49999999999999289 ) ) ;
#562 = CARTESIAN_POINT ( 'NONE',  ( 0.000000000000000000, -1.154700538379251684, -1.199226976249124676E-17 ) ) ;
#563 = DIRECTION ( 'NONE',  ( 0.000000000000000000, 0.000000000000000000, -1.000000000000000000 ) ) ;
#564 = ORIENTED_EDGE ( 'NONE', *, *, #1430, .T. ) ;
#565 = DIRECTION ( 'NONE',  ( 0.000000000000000000, 0.000000000000000000, 1.000000000000000000 ) ) ;
#566 = EDGE_CURVE ( 'NONE', #914, #391, #2569, .T. ) ;
#567 = DIRECTION ( 'NONE',  ( 0.000000000000000000, 0.000000000000000000, 1.000000000000000000 ) ) ;
#568 = FACE_OUTER_BOUND ( 'NONE', #2317, .T. ) ;
#569 = EDGE_LOOP ( 'NONE', ( #1118, #2896, #1520, #1946, #2140 ) ) ;
#570 = DIRECTION ( 'NONE',  ( 1.000000000000000000, 0.000000000000000000, 0.000000000000000000 ) ) ;
#571 = PRODUCT_DEFINITION_CONTEXT ( 'detailed design', #2741, 'design' ) ;
#572 = VERTEX_POINT ( 'NONE', #1304 ) ;
#573 = LINE ( 'NONE', #2313, #957 ) ;
#574 = DIRECTION ( 'NONE',  ( 1.000000000000000000, 0.000000000000000000, 0.000000000000000000 ) ) ;
#575 = EDGE_CURVE ( 'NONE', #2092, #576, #3015, .T. ) ;
#576 = VERTEX_POINT ( 'NONE', #1290 ) ;
#577 = EDGE_LOOP ( 'NONE', ( #3165, #2114 ) ) ;
#578 = CIRCLE ( 'NONE', #2085, 5.000000000000000888 ) ;
#579 = FACE_OUTER_BOUND ( 'NONE', #389, .T. ) ;
#580 = CARTESIAN_POINT ( 'NONE',  ( 1.040000000000000036, 0.5773502691896263972, 1.000000000000000000 ) ) ;
#581 = EDGE_LOOP ( 'NONE', ( #1628, #2886, #1194 ) ) ;
#582 = DIRECTION ( 'NONE',  ( 0.9950371902099894861, 1.218569110023196515E-17, 0.09950371902099541810 ) ) ;
#583 = CYLINDRICAL_SURFACE ( 'NONE', #2281, 10.00000000000000178 ) ;
#584 =( NAMED_UNIT ( * ) PLANE_ANGLE_UNIT ( ) SI_UNIT ( $, .RADIAN. ) );
#585 = VERTEX_POINT ( 'NONE', #1541 ) ;
#586 = CARTESIAN_POINT ( 'NONE',  ( -26.99999999999999645, -5.173438564262573782E-15, 12.49999999999999822 ) ) ;
#587 = ADVANCED_FACE ( 'NONE', ( #1804 ), #785, .F. ) ;
#588 = DIRECTION ( 'NONE',  ( 0.000000000000000000, 0.000000000000000000, -1.000000000000000000 ) ) ;
#589 = ORIENTED_EDGE ( 'NONE', *, *, #610, .T. ) ;
#590 = AXIS2_PLACEMENT_3D ( 'NONE', #2153, #2814, #139 ) ;
#591 = EDGE_CURVE ( 'NONE', #488, #815, #2290, .T. ) ;
#592 = AXIS2_PLACEMENT_3D ( 'NONE', #1852, #1310, #2370 ) ;
#593 = CARTESIAN_POINT ( 'NONE',  ( -30.00000000000000000, -3.673940397442059178E-15, 0.000000000000000000 ) ) ;
#594 = CARTESIAN_POINT ( 'NONE',  ( 7.369500000000001272, 0.000000000000000000, 0.000000000000000000 ) ) ;
#595=STYLED_ITEM('',(#3264),#27);
#596 = ORIENTED_EDGE ( 'NONE', *, *, #1551, .F. ) ;
#597 = CARTESIAN_POINT ( 'NONE',  ( 155.0000000000000284, -5.704195973019200848E-15, -2.500000000000002220 ) ) ;
#598 = EDGE_CURVE ( 'NONE', #1829, #1709, #1645, .T. ) ;
#599 = VECTOR ( 'NONE', #47, 1000.000000000000000 ) ;
#600 = AXIS2_PLACEMENT_3D ( 'NONE', #3063, #77, #3053 ) ;
#601 = DIRECTION ( 'NONE',  ( -0.7071067811865472397, 0.000000000000000000, 0.7071067811865479058 ) ) ;
#602 = ORIENTED_EDGE ( 'NONE', *, *, #1206, .T. ) ;
#603 =( GEOMETRIC_REPRESENTATION_CONTEXT ( 3 ) GLOBAL_UNCERTAINTY_ASSIGNED_CONTEXT ( ( #419 ) ) GLOBAL_UNIT_ASSIGNED_CONTEXT ( ( #2203, #1706, #998 ) ) REPRESENTATION_CONTEXT ( 'NONE', 'WORKASPACE' ) );
#604 = LINE ( 'NONE', #2391, #2518 ) ;
#605 =( LENGTH_UNIT ( ) NAMED_UNIT ( * ) SI_UNIT ( .MILLI., .METRE. ) );
#606 = PLANE ( 'NONE',  #1267 ) ;
#607 = ORIENTED_EDGE ( 'NONE', *, *, #667, .F. ) ;
#608 = CARTESIAN_POINT ( 'NONE',  ( -23.99999999999999645, 4.999999999999994671, 7.500000000000000888 ) ) ;
#609 = CARTESIAN_POINT ( 'NONE',  ( 36.58213974117523293, -6.323013916343274967E-15, 12.50000000000000178 ) ) ;
#610 = EDGE_CURVE ( 'NONE', #531, #1119, #1170, .T. ) ;
#611 = ORIENTED_EDGE ( 'NONE', *, *, #718, .T. ) ;
#612 = CARTESIAN_POINT ( 'NONE',  ( -26.99999999999999645, -5.785761963836251101E-15, 2.500000000000000444 ) ) ;
#613 = AXIS2_PLACEMENT_3D ( 'NONE', #951, #1199, #470 ) ;
#614 = DIRECTION ( 'NONE',  ( 0.000000000000000000, 1.000000000000000000, 0.000000000000000000 ) ) ;
#615 = EDGE_CURVE ( 'NONE', #1621, #241, #2725, .T. ) ;
#616 = DIRECTION ( 'NONE',  ( 1.000000000000000000, 0.000000000000000000, 0.000000000000000000 ) ) ;
#617 = ORIENTED_EDGE ( 'NONE', *, *, #252, .T. ) ;
#618 = CIRCLE ( 'NONE', #2483, 5.000000000000000000 ) ;
#619 = ORIENTED_EDGE ( 'NONE', *, *, #2326, .F. ) ;
#620 = FACE_OUTER_BOUND ( 'NONE', #1333, .T. ) ;
#621 = CARTESIAN_POINT ( 'NONE',  ( 36.58213974117523293, -6.323013916343274967E-15, 12.50000000000000178 ) ) ;
#622 = CIRCLE ( 'NONE', #2438, 1.219500000000000028 ) ;
#623 = CARTESIAN_POINT ( 'NONE',  ( -40.00430309513780003, -9.040569623688697978E-15, 7.500000000000000000 ) ) ;
#624 = EDGE_LOOP ( 'NONE', ( #2555, #789 ) ) ;
#625 = CARTESIAN_POINT ( 'NONE',  ( 37.38775466693719807, 1.452318184980633031, 16.38206869443958169 ) ) ;
#626 = VERTEX_POINT ( 'NONE', #1562 ) ;
#627 = CARTESIAN_POINT ( 'NONE',  ( 140.0000000000000000, -6.316519372592878167E-15, 2.499999999999999556 ) ) ;
#628 = VERTEX_POINT ( 'NONE', #2005 ) ;
#629 = DIRECTION ( 'NONE',  ( -2.312964634635742957E-16, 1.000000000000000000, 0.000000000000000000 ) ) ;
#630 = VECTOR ( 'NONE', #2703, 1000.000000000000000 ) ;
#631 = DIRECTION ( 'NONE',  ( -0.000000000000000000, -0.000000000000000000, -1.000000000000000000 ) ) ;
#632 = DIRECTION ( 'NONE',  ( 0.000000000000000000, 0.000000000000000000, 1.000000000000000000 ) ) ;
#633 =( GEOMETRIC_REPRESENTATION_CONTEXT ( 3 ) GLOBAL_UNCERTAINTY_ASSIGNED_CONTEXT ( ( #2364 ) ) GLOBAL_UNIT_ASSIGNED_CONTEXT ( ( #189, #684, #1683 ) ) REPRESENTATION_CONTEXT ( 'NONE', 'WORKASPACE' ) );
#634 = ORIENTED_EDGE ( 'NONE', *, *, #1634, .T. ) ;
#635 = ORIENTED_EDGE ( 'NONE', *, *, #2964, .T. ) ;
#636 = DIRECTION ( 'NONE',  ( 0.000000000000000000, 0.000000000000000000, -1.000000000000000000 ) ) ;
#637 = ADVANCED_FACE ( 'NONE', ( #2299 ), #812, .F. ) ;
#638 = LINE ( 'NONE', #3137, #2109 ) ;
#639 = LINE ( 'NONE', #1636, #1796 ) ;
#640 = VERTEX_POINT ( 'NONE', #1514 ) ;
#641 = DIRECTION ( 'NONE',  ( 1.000000000000000000, 0.000000000000000000, 0.000000000000000000 ) ) ;
#642 = APPLICATION_CONTEXT ( 'automotive_design' ) ;
#643 = ORIENTED_EDGE ( 'NONE', *, *, #44, .T. ) ;
#644 = DIRECTION ( 'NONE',  ( 0.000000000000000000, 0.000000000000000000, -1.000000000000000000 ) ) ;
#645 = EDGE_LOOP ( 'NONE', ( #2403, #3181 ) ) ;
#646 = PLANE ( 'NONE',  #339 ) ;
#647 = AXIS2_PLACEMENT_3D ( 'NONE', #686, #2975, #2223 ) ;
#648 = CARTESIAN_POINT ( 'NONE',  ( 7.650000000000000355, 0.000000000000000000, 1.219500000000000028 ) ) ;
#649 = CARTESIAN_POINT ( 'NONE',  ( 0.000000000000000000, 0.000000000000000000, 0.000000000000000000 ) ) ;
#650 = CIRCLE ( 'NONE', #1368, 8.999999999999994671 ) ;
#651 = ORIENTED_EDGE ( 'NONE', *, *, #2800, .T. ) ;
#652 = AXIS2_PLACEMENT_3D ( 'NONE', #1966, #1773, #964 ) ;
#653 = FACE_OUTER_BOUND ( 'NONE', #990, .T. ) ;
#654 = AXIS2_PLACEMENT_3D ( 'NONE', #452, #2165, #917 ) ;
#655 = CARTESIAN_POINT ( 'NONE',  ( 37.00000000000000000, 1.474514954580286030E-14, 12.99999999999999822 ) ) ;
#656 = SHAPE_REPRESENTATION_RELATIONSHIP ( 'NONE' , 'NONE' ,  #1116, #1362 ) ;
#657 = EDGE_CURVE ( 'NONE', #1365, #640, #2412, .T. ) ;
#658 = VERTEX_POINT ( 'NONE', #328 ) ;
#659 = DIRECTION ( 'NONE',  ( 0.000000000000000000, 0.000000000000000000, -1.000000000000000000 ) ) ;
#660 = EDGE_CURVE ( 'NONE', #1860, #1904, #1813, .T. ) ;
#661 = ORIENTED_EDGE ( 'NONE', *, *, #1385, .F. ) ;
#662 = DIRECTION ( 'NONE',  ( 1.000000000000000000, 2.312964634635742957E-16, 0.000000000000000000 ) ) ;
#663 = ORIENTED_EDGE ( 'NONE', *, *, #843, .F. ) ;
#664 = CARTESIAN_POINT ( 'NONE',  ( 37.00000000000000000, 1.474514954580286030E-14, 20.99999999999999645 ) ) ;
#665 = EDGE_LOOP ( 'NONE', ( #1180, #1453, #1135, #836 ) ) ;
#666 = CARTESIAN_POINT ( 'NONE',  ( 155.0000000000000284, -6.928842772166554697E-15, 7.500000000000000000 ) ) ;
#667 = EDGE_CURVE ( 'NONE', #531, #3100, #2993, .T. ) ;
#668 = LINE ( 'NONE', #730, #1764 ) ;
#669 = ORIENTED_EDGE ( 'NONE', *, *, #1688, .T. ) ;
#670 = SURFACE_STYLE_USAGE ( .BOTH. , #2897 ) ;
#671 = EDGE_CURVE ( 'NONE', #1489, #1964, #2710, .T. ) ;
#672 = CARTESIAN_POINT ( 'NONE',  ( 155.0000000000000284, -6.928842772166554697E-15, 7.500000000000000000 ) ) ;
#673 = VECTOR ( 'NONE', #1742, 1000.000000000000000 ) ;
#674 = CARTESIAN_POINT ( 'NONE',  ( 87.00000000000000000, -7.622732162557277534E-15, 7.500000000000000000 ) ) ;
#675 = ORIENTED_EDGE ( 'NONE', *, *, #1886, .F. ) ;
#676 = CARTESIAN_POINT ( 'NONE',  ( 35.68903409116789049, 0.7546922429561601087, 16.47012649564898368 ) ) ;
#677 = EDGE_CURVE ( 'NONE', #861, #1621, #573, .T. ) ;
#678 = ORIENTED_EDGE ( 'NONE', *, *, #3014, .F. ) ;
#679 = PLANE ( 'NONE',  #1059 ) ;
#680 = ORIENTED_EDGE ( 'NONE', *, *, #2129, .T. ) ;
#681 = DIRECTION ( 'NONE',  ( 0.000000000000000000, 1.000000000000000000, 0.000000000000000000 ) ) ;
#682 = CARTESIAN_POINT ( 'NONE',  ( 30.00000000000000355, -11.82159041753688200, 15.00000000000000000 ) ) ;
#683 = DIRECTION ( 'NONE',  ( 0.000000000000000000, 0.000000000000000000, 1.000000000000000000 ) ) ;
#684 =( NAMED_UNIT ( * ) PLANE_ANGLE_UNIT ( ) SI_UNIT ( $, .RADIAN. ) );
#685 = DIRECTION ( 'NONE',  ( 0.000000000000000000, 0.000000000000000000, 1.000000000000000000 ) ) ;
#686 = CARTESIAN_POINT ( 'NONE',  ( 3.469446951953614189E-15, -15.00000000000000355, 15.00000000000000000 ) ) ;
#687 = ORIENTED_EDGE ( 'NONE', *, *, #1176, .F. ) ;
#688 = AXIS2_PLACEMENT_3D ( 'NONE', #503, #2415, #965 ) ;
#689 = CARTESIAN_POINT ( 'NONE',  ( 35.50000000000000000, -7.622732095468789599E-15, 16.49999999999999289 ) ) ;
#690 = EDGE_LOOP ( 'NONE', ( #13, #3111, #3143, #1378, #349, #2589 ) ) ;
#691 = ORIENTED_EDGE ( 'NONE', *, *, #1656, .T. ) ;
#692 = EDGE_CURVE ( 'NONE', #3085, #1246, #230, .T. ) ;
#693 = CARTESIAN_POINT ( 'NONE',  ( -37.00000000000000000, -5.785761963836251101E-15, 2.500000000000001332 ) ) ;
#694 = PRODUCT_DEFINITION ( 'UNKNOWN', '', #708, #307 ) ;
#695 = CARTESIAN_POINT ( 'NONE',  ( -29.99999999999999645, -15.00000000000000355, 15.00000000000000000 ) ) ;
#696 = CARTESIAN_POINT ( 'NONE',  ( 87.00000000000000000, -7.010408762983600216E-15, 2.499999999999999556 ) ) ;
#697 = COLOUR_RGB ( '',0.8941176470588234615, 0.8941176470588234615, 0.8941176470588234615 ) ;
#698 = FACE_OUTER_BOUND ( 'NONE', #2603, .T. ) ;
#699 = CLOSED_SHELL ( 'NONE', ( #2287, #1331, #2040, #2558, #1386, #1530, #475, #2835, #165, #637, #795, #1234, #1613 ) ) ;
#700 = DIRECTION ( 'NONE',  ( 1.000000000000000000, 0.000000000000000000, 0.000000000000000000 ) ) ;
#701 = AXIS2_PLACEMENT_3D ( 'NONE', #3218, #2792, #1016 ) ;
#702 = VECTOR ( 'NONE', #227, 1000.000000000000000 ) ;
#703 = AXIS2_PLACEMENT_3D ( 'NONE', #1569, #2144, #2570 ) ;
#704 = VECTOR ( 'NONE', #1350, 1000.000000000000000 ) ;
#705 = COLOUR_RGB ( '',0.8941176470588234615, 0.8941176470588234615, 0.8941176470588234615 ) ;
#706 = LINE ( 'NONE', #474, #2158 ) ;
#707 = DIRECTION ( 'NONE',  ( -0.000000000000000000, -0.5000000000000000000, 0.8660254037844385966 ) ) ;
#708 = PRODUCT_DEFINITION_FORMATION_WITH_SPECIFIED_SOURCE ( 'ANY', '', #2285, .NOT_KNOWN. ) ;
#709 = ORIENTED_EDGE ( 'NONE', *, *, #2679, .T. ) ;
#710 = DIRECTION ( 'NONE',  ( 1.000000000000000000, -0.000000000000000000, -0.000000000000000000 ) ) ;
#711 = ORIENTED_EDGE ( 'NONE', *, *, #1812, .F. ) ;
#712 = DIRECTION ( 'NONE',  ( 1.000000000000000000, 0.000000000000000000, 0.000000000000000000 ) ) ;
#713 = EDGE_CURVE ( 'NONE', #1393, #3128, #2675, .T. ) ;
#714 = CYLINDRICAL_SURFACE ( 'NONE', #1903, 9.000000000000001776 ) ;
#715 = CARTESIAN_POINT ( 'NONE',  ( 140.0000000000000000, -6.316519372592878167E-15, 2.499999999999999556 ) ) ;
#716 = DIRECTION ( 'NONE',  ( 0.000000000000000000, 1.000000000000000000, 1.224646799147353207E-16 ) ) ;
#717 = DIRECTION ( 'NONE',  ( 0.000000000000000000, 0.000000000000000000, 1.000000000000000000 ) ) ;
#718 = EDGE_CURVE ( 'NONE', #310, #1076, #275, .T. ) ;
#719 = DIRECTION ( 'NONE',  ( -1.000000000000000000, 0.000000000000000000, -0.000000000000000000 ) ) ;
#720 = SURFACE_SIDE_STYLE ('',( #205 ) ) ;
#721 = EDGE_CURVE ( 'NONE', #1182, #169, #2268, .T. ) ;
#722 = AXIS2_PLACEMENT_3D ( 'NONE', #2605, #1834, #113 ) ;
#723 = CARTESIAN_POINT ( 'NONE',  ( 87.00000000000000000, -6.520550043324660412E-15, -1.499999999999992673 ) ) ;
#724 = CARTESIAN_POINT ( 'NONE',  ( 1.269999999999999796, -2.850000000000000533, -3.490243377569956061E-16 ) ) ;
#725 = ORIENTED_EDGE ( 'NONE', *, *, #2852, .F. ) ;
#726 = ORIENTED_EDGE ( 'NONE', *, *, #2442, .F. ) ;
#727 = DIRECTION ( 'NONE',  ( 0.000000000000000000, 1.000000000000000000, 0.000000000000000000 ) ) ;
#728 = CARTESIAN_POINT ( 'NONE',  ( 100.0000000000000000, -5.459266613189731341E-15, -4.500000000000000888 ) ) ;
#729 = FACE_OUTER_BOUND ( 'NONE', #989, .T. ) ;
#730 = CARTESIAN_POINT ( 'NONE',  ( 30.00000000000000355, -15.00000000000000355, 15.00000000000000000 ) ) ;
#731 = EDGE_CURVE ( 'NONE', #548, #738, #541, .T. ) ;
#732 = DIRECTION ( 'NONE',  ( 1.000000000000000000, 2.312964634635742957E-16, 0.000000000000000000 ) ) ;
#733 = EDGE_CURVE ( 'NONE', #2373, #626, #638, .T. ) ;
#734 = CARTESIAN_POINT ( 'NONE',  ( 38.25000000000000000, 1.474514954580286030E-14, 12.99999999999999822 ) ) ;
#735 = EDGE_CURVE ( 'NONE', #572, #1823, #604, .T. ) ;
#736 = CARTESIAN_POINT ( 'NONE',  ( 41.99999999999999289, -11.82159041753688022, 0.000000000000000000 ) ) ;
#737 = ORIENTED_EDGE ( 'NONE', *, *, #1525, .T. ) ;
#738 = VERTEX_POINT ( 'NONE', #1122 ) ;
#739 = AXIS2_PLACEMENT_3D ( 'NONE', #3054, #318, #567 ) ;
#740 = CARTESIAN_POINT ( 'NONE',  ( 140.0000000000000000, -6.928842772166554697E-15, 20.50000000000000000 ) ) ;
#741 = FACE_OUTER_BOUND ( 'NONE', #2868, .T. ) ;
#742 = CARTESIAN_POINT ( 'NONE',  ( 37.36887240208277916, -0.2104090322588208772, 12.49607929530250239 ) ) ;
#743 = CONTEXT_DEPENDENT_SHAPE_REPRESENTATION ( #2506, #222 ) ;
#744 = PLANE ( 'NONE',  #1838 ) ;
#745 = VERTEX_POINT ( 'NONE', #154 ) ;
#746 = VECTOR ( 'NONE', #732, 1000.000000000000000 ) ;
#747 = AXIS2_PLACEMENT_3D ( 'NONE', #194, #1501, #208 ) ;
#748 = EDGE_CURVE ( 'NONE', #79, #3095, #2563, .T. ) ;
#749 = DIRECTION ( 'NONE',  ( 0.000000000000000000, 0.000000000000000000, 1.000000000000000000 ) ) ;
#750 = DIRECTION ( 'NONE',  ( -0.000000000000000000, -0.000000000000000000, -1.000000000000000000 ) ) ;
#751 = AXIS2_PLACEMENT_3D ( 'NONE', #312, #39, #294 ) ;
#752 = ORIENTED_EDGE ( 'NONE', *, *, #2047, .F. ) ;
#753 = ORIENTED_EDGE ( 'NONE', *, *, #1619, .F. ) ;
#754 = AXIS2_PLACEMENT_3D ( 'NONE', #2606, #135, #388 ) ;
#755 = CARTESIAN_POINT ( 'NONE',  ( -5.000000000000000000, -6.928842772166554697E-15, 7.500000000000000000 ) ) ;
#756 = CARTESIAN_POINT ( 'NONE',  ( -37.00000000000000000, -5.173438564262574571E-15, 12.49999999999999645 ) ) ;
#757 = PLANE ( 'NONE',  #2282 ) ;
#758 = PRODUCT_DEFINITION_FORMATION_WITH_SPECIFIED_SOURCE ( 'ANY', '', #2237, .NOT_KNOWN. ) ;
#759 = EDGE_CURVE ( 'NONE', #626, #2346, #3103, .T. ) ;
#760 = DIRECTION ( 'NONE',  ( -1.000000000000000000, -0.000000000000000000, -0.000000000000000000 ) ) ;
#761 = EDGE_CURVE ( 'NONE', #3197, #2355, #2875, .T. ) ;
#762 = DIRECTION ( 'NONE',  ( 1.000000000000000000, 0.000000000000000000, 0.000000000000000000 ) ) ;
#763 = ORIENTED_EDGE ( 'NONE', *, *, #270, .F. ) ;
#764 = DIRECTION ( 'NONE',  ( 1.000000000000000000, 0.000000000000000000, 0.000000000000000000 ) ) ;
#765 = CARTESIAN_POINT ( 'NONE',  ( 1.649999999999999911, 0.000000000000000000, 0.000000000000000000 ) ) ;
#766 = DIRECTION ( 'NONE',  ( 1.000000000000000000, 0.000000000000000000, 0.000000000000000000 ) ) ;
#767 = AXIS2_PLACEMENT_3D ( 'NONE', #1954, #2911, #683 ) ;
#768 = ORIENTED_EDGE ( 'NONE', *, *, #610, .F. ) ;
#769 = AXIS2_PLACEMENT_3D ( 'NONE', #3204, #435, #2416 ) ;
#770 = VERTEX_POINT ( 'NONE', #1596 ) ;
#771 = ADVANCED_FACE ( 'NONE', ( #2358 ), #1893, .T. ) ;
#772 = EDGE_CURVE ( 'NONE', #1678, #1779, #333, .T. ) ;
#773 = DIRECTION ( 'NONE',  ( 1.000000000000000000, 2.312964634635742957E-16, 0.000000000000000000 ) ) ;
#774 = DIRECTION ( 'NONE',  ( 1.000000000000000000, 2.312964634635742957E-16, -0.000000000000000000 ) ) ;
#775 = DIRECTION ( 'NONE',  ( 1.000000000000000000, 0.000000000000000000, 0.000000000000000000 ) ) ;
#776 =( LENGTH_UNIT ( ) NAMED_UNIT ( * ) SI_UNIT ( .MILLI., .METRE. ) );
#777 = UNCERTAINTY_MEASURE_WITH_UNIT (LENGTH_MEASURE( 1.000000000000000082E-05 ), #1533, 'distance_accuracy_value', 'NONE');
#778 = CARTESIAN_POINT ( 'NONE',  ( -41.99999999999999289, -1.109217911451089172E-14, 7.500000000000000000 ) ) ;
#779 = VERTEX_POINT ( 'NONE', #586 ) ;
#780 = DIRECTION ( 'NONE',  ( -1.000000000000000000, -0.000000000000000000, -0.000000000000000000 ) ) ;
#781 = CARTESIAN_POINT ( 'NONE',  ( 27.00000000000000000, 6.704247063196759979E-15, 7.500000000000000000 ) ) ;
#782 = CARTESIAN_POINT ( 'NONE',  ( -26.99999999999999645, -5.785761963836251101E-15, 7.500000000000000000 ) ) ;
#783 = FILL_AREA_STYLE ('',( #1272 ) ) ;
#784 = ORIENTED_EDGE ( 'NONE', *, *, #2418, .T. ) ;
#785 = CYLINDRICAL_SURFACE ( 'NONE', #395, 5.000000000000000888 ) ;
#786 = DIRECTION ( 'NONE',  ( -0.7071067811865472397, 8.659560562354937789E-17, -0.7071067811865479058 ) ) ;
#787 = CARTESIAN_POINT ( 'NONE',  ( 37.41786025882473865, -0.1064896851603509553, 12.50000000000000178 ) ) ;
#788 = ADVANCED_FACE ( 'NONE', ( #1081 ), #2634, .T. ) ;
#789 = ORIENTED_EDGE ( 'NONE', *, *, #337, .T. ) ;
#790 = AXIS2_PLACEMENT_3D ( 'NONE', #2216, #1953, #2198 ) ;
#791 = CARTESIAN_POINT ( 'NONE',  ( 1.750000000000000000, 0.000000000000000000, 0.000000000000000000 ) ) ;
#792 = LINE ( 'NONE', #2780, #2329 ) ;
#793 =( NAMED_UNIT ( * ) SI_UNIT ( $, .STERADIAN. ) SOLID_ANGLE_UNIT ( ) );
#794 = ORIENTED_EDGE ( 'NONE', *, *, #28, .T. ) ;
#795 = ADVANCED_FACE ( 'NONE', ( #2578 ), #1099, .F. ) ;
#796 = CARTESIAN_POINT ( 'NONE',  ( 35.54829862735515889, 0.3901384415568778796, 16.49205630963118807 ) ) ;
#797 = CIRCLE ( 'NONE', #2874, 8.999999999999992895 ) ;
#798 = DIRECTION ( 'NONE',  ( 1.000000000000000000, 0.000000000000000000, 0.000000000000000000 ) ) ;
#799 = EDGE_CURVE ( 'NONE', #1823, #2935, #1473, .T. ) ;
#800 = CARTESIAN_POINT ( 'NONE',  ( 155.0000000000000284, -6.928842772166554697E-15, 12.50000000000000000 ) ) ;
#801 =( GEOMETRIC_REPRESENTATION_CONTEXT ( 3 ) GLOBAL_UNCERTAINTY_ASSIGNED_CONTEXT ( ( #1879 ) ) GLOBAL_UNIT_ASSIGNED_CONTEXT ( ( #776, #1509, #3040 ) ) REPRESENTATION_CONTEXT ( 'NONE', 'WORKASPACE' ) );
#802 = ORIENTED_EDGE ( 'NONE', *, *, #575, .T. ) ;
#803 = VECTOR ( 'NONE', #2318, 1000.000000000000227 ) ;
#804 = DIRECTION ( 'NONE',  ( 0.000000000000000000, -1.000000000000000000, 0.000000000000000000 ) ) ;
#805 = CARTESIAN_POINT ( 'NONE',  ( 35.75000000000000000, 1.489823039569627924E-14, 13.99999999999999822 ) ) ;
#806 = DIRECTION ( 'NONE',  ( 1.000000000000000000, 0.000000000000000000, 0.000000000000000000 ) ) ;
#807 = ORIENTED_EDGE ( 'NONE', *, *, #1490, .T. ) ;
#808 = APPLICATION_CONTEXT ( 'automotive_design' ) ;
#809 = COLOUR_RGB ( '',0.8941176470588234615, 0.8941176470588234615, 0.8941176470588234615 ) ;
#810 = ORIENTED_EDGE ( 'NONE', *, *, #517, .F. ) ;
#811 = EDGE_CURVE ( 'NONE', #546, #1226, #543, .T. ) ;
#812 = CYLINDRICAL_SURFACE ( 'NONE', #751, 1.499999999999994449 ) ;
#813 = CARTESIAN_POINT ( 'NONE',  ( 1.269999999999999796, 0.000000000000000000, 0.000000000000000000 ) ) ;
#814 = CARTESIAN_POINT ( 'NONE',  ( 1.040000000000000036, -1.154700538379251684, 0.000000000000000000 ) ) ;
#815 = VERTEX_POINT ( 'NONE', #872 ) ;
#816 = LINE ( 'NONE', #3033, #704 ) ;
#817 = AXIS2_PLACEMENT_3D ( 'NONE', #2148, #3132, #1968 ) ;
#818 = LINE ( 'NONE', #756, #599 ) ;
#819 = ORIENTED_EDGE ( 'NONE', *, *, #1576, .T. ) ;
#820 = DIRECTION ( 'NONE',  ( -0.000000000000000000, -0.5000000000000003331, -0.8660254037844383745 ) ) ;
#821 = DIRECTION ( 'NONE',  ( 0.000000000000000000, 0.000000000000000000, 1.000000000000000000 ) ) ;
#822 = SURFACE_STYLE_FILL_AREA ( #2068 ) ;
#823 = ORIENTED_EDGE ( 'NONE', *, *, #2248, .T. ) ;
#824 = ADVANCED_BREP_SHAPE_REPRESENTATION ( '', ( #27, #2878 ), #1010 ) ;
#825 = CARTESIAN_POINT ( 'NONE',  ( 35.80758137781341333, 0.9152444266664423456, 16.45371270176149991 ) ) ;
#826 = FILL_AREA_STYLE_COLOUR ( '', #63 ) ;
#827 = ADVANCED_FACE ( 'NONE', ( #1578 ), #3119, .T. ) ;
#828 = PRODUCT_RELATED_PRODUCT_CATEGORY ( 'part', '', ( #2771 ) ) ;
#829 = ADVANCED_FACE ( 'NONE', ( #1330, #2376 ), #1614, .T. ) ;
#830 = ORIENTED_EDGE ( 'NONE', *, *, #2211, .T. ) ;
#831 = CARTESIAN_POINT ( 'NONE',  ( -23.99999999999999645, -5.000000000000007994, 7.500000000000000000 ) ) ;
#832 = LINE ( 'NONE', #2833, #2937 ) ;
#833 = ORIENTED_EDGE ( 'NONE', *, *, #2536, .F. ) ;
#834 = CARTESIAN_POINT ( 'NONE',  ( 27.00000000000000000, 1.133017633246824530E-14, 7.500000000000000000 ) ) ;
#835 = DIRECTION ( 'NONE',  ( 1.000000000000000000, 2.312964634635742957E-16, 0.000000000000000000 ) ) ;
#836 = ORIENTED_EDGE ( 'NONE', *, *, #2343, .F. ) ;
#837 = DIRECTION ( 'NONE',  ( -0.000000000000000000, -0.000000000000000000, -1.000000000000000000 ) ) ;
#838 = LINE ( 'NONE', #2784, #2614 ) ;
#839 = EDGE_CURVE ( 'NONE', #1877, #916, #3032, .T. ) ;
#840 = ORIENTED_EDGE ( 'NONE', *, *, #1067, .T. ) ;
#841 = EDGE_LOOP ( 'NONE', ( #929, #2082, #634, #2585 ) ) ;
#842 = AXIS2_PLACEMENT_3D ( 'NONE', #2187, #3172, #938 ) ;
#843 = EDGE_CURVE ( 'NONE', #2350, #2807, #1836, .T. ) ;
#844 = VECTOR ( 'NONE', #820, 1000.000000000000114 ) ;
#845 = CARTESIAN_POINT ( 'NONE',  ( 35.50000000000000000, 1.492884656567496302E-14, 13.99999999999999822 ) ) ;
#846 = CARTESIAN_POINT ( 'NONE',  ( -29.99999999999999645, -15.00000000000000355, 15.00000000000000000 ) ) ;
#847 = ORIENTED_EDGE ( 'NONE', *, *, #1892, .F. ) ;
#848 = CARTESIAN_POINT ( 'NONE',  ( 0.000000000000000000, 0.5773502691896263972, -1.000000000000000000 ) ) ;
#849 = CIRCLE ( 'NONE', #2056, 9.000000000000000000 ) ;
#850 = AXIS2_PLACEMENT_3D ( 'NONE', #2539, #2547, #764 ) ;
#851 = FACE_OUTER_BOUND ( 'NONE', #1488, .T. ) ;
#852 = PRESENTATION_LAYER_ASSIGNMENT (  '', '', ( #2940 ) ) ;
#853 = DIRECTION ( 'NONE',  ( 0.000000000000000000, 0.000000000000000000, 1.000000000000000000 ) ) ;
#854 = EDGE_LOOP ( 'NONE', ( #691, #589 ) ) ;
#855 = ORIENTED_EDGE ( 'NONE', *, *, #1308, .T. ) ;
#856 = DIRECTION ( 'NONE',  ( -1.000000000000000000, -2.312964634635742957E-16, -0.000000000000000000 ) ) ;
#857 = PLANE ( 'NONE',  #1367 ) ;
#858 = EDGE_LOOP ( 'NONE', ( #30, #819 ) ) ;
#859 = ORIENTED_EDGE ( 'NONE', *, *, #1403, .F. ) ;
#860 = DIRECTION ( 'NONE',  ( 1.000000000000000000, 0.000000000000000000, 0.000000000000000000 ) ) ;
#861 = VERTEX_POINT ( 'NONE', #621 ) ;
#862 = ADVANCED_FACE ( 'NONE', ( #2594, #2858 ), #1684, .T. ) ;
#863 = CARTESIAN_POINT ( 'NONE',  ( 140.0000000000000000, -6.928842772166554697E-15, 12.50000000000000000 ) ) ;
#864 = CIRCLE ( 'NONE', #81, 7.500000000000000000 ) ;
#866 = EDGE_CURVE ( 'NONE', #106, #137, #2406, .T. ) ;
#865 = DIRECTION ( 'NONE',  ( 0.000000000000000000, 0.000000000000000000, 1.000000000000000000 ) ) ;
#867 = DIRECTION ( 'NONE',  ( 1.000000000000000000, 0.000000000000000000, 0.000000000000000000 ) ) ;
#868 = ORIENTED_EDGE ( 'NONE', *, *, #2571, .F. ) ;
#869 = VECTOR ( 'NONE', #662, 1000.000000000000000 ) ;
#870 = ORIENTED_EDGE ( 'NONE', *, *, #1061, .T. ) ;
#871 = FACE_OUTER_BOUND ( 'NONE', #3146, .T. ) ;
#872 = CARTESIAN_POINT ( 'NONE',  ( 1.750000000000000000, 0.000000000000000000, 1.499999999999999556 ) ) ;
#873 = UNCERTAINTY_MEASURE_WITH_UNIT (LENGTH_MEASURE( 1.000000000000000082E-05 ), #3007, 'distance_accuracy_value', 'NONE');
#874 = CARTESIAN_POINT ( 'NONE',  ( 47.00000000000000000, -13.99999999999998757, 7.500000000000001776 ) ) ;
#875 = EDGE_LOOP ( 'NONE', ( #768, #1279, #2791, #1807 ) ) ;
#876 = CARTESIAN_POINT ( 'NONE',  ( 38.49999999999999289, -7.622732162557277534E-15, 16.49999999999999289 ) ) ;
#877 = VERTEX_POINT ( 'NONE', #2663 ) ;
#878 = CARTESIAN_POINT ( 'NONE',  ( 155.0000000000000284, -6.928842772166554697E-15, 7.500000000000000000 ) ) ;
#879 = EDGE_LOOP ( 'NONE', ( #2061, #2408 ) ) ;
#880 = DIRECTION ( 'NONE',  ( 1.000000000000000000, 2.312964634635742957E-16, 0.000000000000000000 ) ) ;
#881=STYLED_ITEM('',(#3250),#2099);
#882 = EDGE_CURVE ( 'NONE', #1076, #1030, #797, .T. ) ;
#883 = CARTESIAN_POINT ( 'NONE',  ( 47.00000000000000000, 1.133017633246824530E-14, 7.500000000000000000 ) ) ;
#884 = CARTESIAN_POINT ( 'NONE',  ( 0.000000000000000000, 0.000000000000000000, 0.000000000000000000 ) ) ;
#885 = EDGE_LOOP ( 'NONE', ( #2107, #555, #2207 ) ) ;
#886 = EDGE_LOOP ( 'NONE', ( #2902, #3101, #2704, #146, #2952 ) ) ;
#887 = CARTESIAN_POINT ( 'NONE',  ( 1.617350269189632428, 0.000000000000000000, 0.000000000000000000 ) ) ;
#888 = DIRECTION ( 'NONE',  ( -0.000000000000000000, -0.5000000000000000000, 0.8660254037844385966 ) ) ;
#889 = CARTESIAN_POINT ( 'NONE',  ( 0.000000000000000000, 0.000000000000000000, 0.000000000000000000 ) ) ;
#890 = AXIS2_PLACEMENT_3D ( 'NONE', #2030, #2540, #1759 ) ;
#891 = DIRECTION ( 'NONE',  ( 0.000000000000000000, -0.8660254037844387076, -0.5000000000000001110 ) ) ;
#892 = ORIENTED_EDGE ( 'NONE', *, *, #1433, .T. ) ;
#893 = EDGE_CURVE ( 'NONE', #2713, #2821, #204, .T. ) ;
#894 = CARTESIAN_POINT ( 'NONE',  ( 150.0000000000000000, -6.928842772166554697E-15, 7.500000000000000000 ) ) ;
#895 = ORIENTED_EDGE ( 'NONE', *, *, #314, .T. ) ;
#896 = CARTESIAN_POINT ( 'NONE',  ( 37.41786025882475286, 0.1065494216233999342, 12.50000000000000000 ) ) ;
#897 = ORIENTED_EDGE ( 'NONE', *, *, #2211, .F. ) ;
#898 = CIRCLE ( 'NONE', #1363, 5.000000000000000000 ) ;
#899 = CARTESIAN_POINT ( 'NONE',  ( 87.00000000000000000, -7.622732162557277534E-15, 7.500000000000000000 ) ) ;
#900 = AXIS2_PLACEMENT_3D ( 'NONE', #2362, #363, #3105 ) ;
#901 = COLOUR_RGB ( '',0.8941176470588234615, 0.8941176470588234615, 0.8941176470588234615 ) ;
#902 = CARTESIAN_POINT ( 'NONE',  ( 87.00000000000000000, -7.622732162557277534E-15, 12.50000000000000000 ) ) ;
#903 = PRODUCT_CONTEXT ( 'NONE', #969, 'mechanical' ) ;
#904 = AXIS2_PLACEMENT_3D ( 'NONE', #2849, #2602, #1075 ) ;
#905 = ORIENTED_EDGE ( 'NONE', *, *, #1329, .F. ) ;
#906 = AXIS2_PLACEMENT_3D ( 'NONE', #1555, #2527, #46 ) ;
#907 = PRODUCT_DEFINITION_SHAPE ( 'NONE', 'NONE',  #254 ) ;
#908 = DIRECTION ( 'NONE',  ( 0.000000000000000000, 0.000000000000000000, -1.000000000000000000 ) ) ;
#909 = EDGE_CURVE ( 'NONE', #106, #211, #3189, .T. ) ;
#910 = COLOUR_RGB ( '',0.8941176470588234615, 0.8941176470588234615, 0.8941176470588234615 ) ;
#911 = FACE_OUTER_BOUND ( 'NONE', #2074, .T. ) ;
#912 = ORIENTED_EDGE ( 'NONE', *, *, #2361, .F. ) ;
#913 = LINE ( 'NONE', #126, #3161 ) ;
#914 = VERTEX_POINT ( 'NONE', #1705 ) ;
#915 = DIRECTION ( 'NONE',  ( -0.000000000000000000, -0.000000000000000000, 1.000000000000000000 ) ) ;
#916 = VERTEX_POINT ( 'NONE', #440 ) ;
#917 = DIRECTION ( 'NONE',  ( 0.000000000000000000, -1.000000000000000000, 0.000000000000000000 ) ) ;
#918 = CARTESIAN_POINT ( 'NONE',  ( -26.99999999999999645, -5.785761963836251101E-15, 7.500000000000000000 ) ) ;
#919 = DIRECTION ( 'NONE',  ( -1.000000000000000000, -0.000000000000000000, -0.000000000000000000 ) ) ;
#920 = CARTESIAN_POINT ( 'NONE',  ( 37.00000000000000000, 1.474514954580286030E-14, 22.64999999999999503 ) ) ;
#921 = EDGE_LOOP ( 'NONE', ( #2765, #975 ) ) ;
#922 = PRESENTATION_STYLE_ASSIGNMENT (( #170 ) ) ;
#923 = CIRCLE ( 'NONE', #1970, 1.000000000000000000 ) ;
#924 = CARTESIAN_POINT ( 'NONE',  ( 27.00000000000000355, -11.82159041753688200, 15.00000000000000000 ) ) ;
#925 =( NAMED_UNIT ( * ) PLANE_ANGLE_UNIT ( ) SI_UNIT ( $, .RADIAN. ) );
#926 = CIRCLE ( 'NONE', #462, 1.599999999999999645 ) ;
#927 = EDGE_CURVE ( 'NONE', #1944, #2825, #1216, .T. ) ;
#928 = CARTESIAN_POINT ( 'NONE',  ( 1.040000000000000036, -1.154700538379251684, 0.000000000000000000 ) ) ;
#929 = ORIENTED_EDGE ( 'NONE', *, *, #1865, .F. ) ;
#930 = CARTESIAN_POINT ( 'NONE',  ( 52.00000000000000711, 3.708099243547853252, 20.99999999999999645 ) ) ;
#931 = EDGE_CURVE ( 'NONE', #1570, #585, #2261, .T. ) ;
#932 = ORIENTED_EDGE ( 'NONE', *, *, #1576, .F. ) ;
#933 = ORIENTED_EDGE ( 'NONE', *, *, #2759, .F. ) ;
#934 = CARTESIAN_POINT ( 'NONE',  ( 7.650000000000000355, 0.000000000000000000, 0.000000000000000000 ) ) ;
#935 = DIRECTION ( 'NONE',  ( -0.000000000000000000, -1.000000000000000000, -0.000000000000000000 ) ) ;
#936 = DIRECTION ( 'NONE',  ( -1.000000000000000000, -0.000000000000000000, -0.000000000000000000 ) ) ;
#937 = PRESENTATION_STYLE_ASSIGNMENT (( #2914 ) ) ;
#938 = DIRECTION ( 'NONE',  ( 0.000000000000000000, 0.000000000000000000, 1.000000000000000000 ) ) ;
#939 = AXIS2_PLACEMENT_3D ( 'NONE', #1517, #463, #766 ) ;
#940 = CARTESIAN_POINT ( 'NONE',  ( 180.0000000000000284, -5.704195973019200848E-15, -2.500000000000002220 ) ) ;
#941 = AXIS2_PLACEMENT_3D ( 'NONE', #1146, #2146, #3131 ) ;
#942 = CARTESIAN_POINT ( 'NONE',  ( 38.45998082922277916, 0.3957415549423320411, 16.49311123862705486 ) ) ;
#943 = EDGE_CURVE ( 'NONE', #2713, #357, #3155, .T. ) ;
#944 = ORIENTED_EDGE ( 'NONE', *, *, #1085, .F. ) ;
#945 = PRESENTATION_STYLE_ASSIGNMENT (( #2690 ) ) ;
#946 = ORIENTED_EDGE ( 'NONE', *, *, #234, .F. ) ;
#947 = EDGE_CURVE ( 'NONE', #2850, #815, #2610, .T. ) ;
#948 = DIRECTION ( 'NONE',  ( 0.000000000000000000, 0.000000000000000000, 1.000000000000000000 ) ) ;
#949 = CARTESIAN_POINT ( 'NONE',  ( 38.50000000000000711, -0.09929498707317854778, 16.49999999999999645 ) ) ;
#950 = LINE ( 'NONE', #1211, #1940 ) ;
#951 = CARTESIAN_POINT ( 'NONE',  ( -37.00000000000000000, -5.785761963836251101E-15, 7.500000000000000000 ) ) ;
#952 = SHAPE_DEFINITION_REPRESENTATION ( #119, #1116 ) ;
#953 = FILL_AREA_STYLE ('',( #2417 ) ) ;
#954 = CIRCLE ( 'NONE', #1215, 5.000000000000000000 ) ;
#955 = DIRECTION ( 'NONE',  ( -1.000000000000000000, -0.000000000000000000, -0.000000000000000000 ) ) ;
#956 = VECTOR ( 'NONE', #1905, 1000.000000000000000 ) ;
#957 = VECTOR ( 'NONE', #1500, 1000.000000000000000 ) ;
#958 = CARTESIAN_POINT ( 'NONE',  ( 180.0000000000000284, -6.928842772166554697E-15, 17.50000000000000000 ) ) ;
#959 = PRESENTATION_LAYER_ASSIGNMENT (  '', '', ( #2677 ) ) ;
#960 = PLANE ( 'NONE',  #1825 ) ;
#961 = ORIENTED_EDGE ( 'NONE', *, *, #2571, .T. ) ;
#962 = ORIENTED_EDGE ( 'NONE', *, *, #893, .T. ) ;
#963 = FACE_OUTER_BOUND ( 'NONE', #1238, .T. ) ;
#964 = DIRECTION ( 'NONE',  ( 0.000000000000000000, 0.000000000000000000, -1.000000000000000000 ) ) ;
#965 = DIRECTION ( 'NONE',  ( 0.000000000000000000, 0.000000000000000000, 1.000000000000000000 ) ) ;
#966 = FACE_OUTER_BOUND ( 'NONE', #1512, .T. ) ;
#967 = ADVANCED_FACE ( 'NONE', ( #2453 ), #2960, .F. ) ;
#968 = DIRECTION ( 'NONE',  ( 0.000000000000000000, 0.000000000000000000, 1.000000000000000000 ) ) ;
#969 = APPLICATION_CONTEXT ( 'automotive_design' ) ;
#970 = DIRECTION ( 'NONE',  ( 0.9950371902099894861, 0.000000000000000000, -0.09950371902099541810 ) ) ;
#971 = CONICAL_SURFACE ( 'NONE', #2796, 1732.050807568857181, 1.047197551196592746 ) ;
#972 = CARTESIAN_POINT ( 'NONE',  ( 0.000000000000000000, 1.836970198721029441E-16, -1.499999999999999556 ) ) ;
#973 = CARTESIAN_POINT ( 'NONE',  ( 41.99999999999999289, -15.00000000000000355, 15.00000000000000000 ) ) ;
#974 = VERTEX_POINT ( 'NONE', #1187 ) ;
#975 = ORIENTED_EDGE ( 'NONE', *, *, #274, .F. ) ;
#976 = CARTESIAN_POINT ( 'NONE',  ( 38.30162487582175856, -0.7519129166725451174, 16.46890859085320002 ) ) ;
#977 = DIRECTION ( 'NONE',  ( 0.000000000000000000, -0.5000000000000003331, 0.8660254037844383745 ) ) ;
#978 = CARTESIAN_POINT ( 'NONE',  ( -30.00000000000000000, -7.500000000000007994, 7.500000000000000000 ) ) ;
#979 = ITEM_DEFINED_TRANSFORMATION ( 'NONE', 'NONE', #1485,  #2878 ) ;
#980 = DIRECTION ( 'NONE',  ( 0.000000000000000000, 0.000000000000000000, -1.000000000000000000 ) ) ;
#981 = EDGE_CURVE ( 'NONE', #2037, #479, #1478, .T. ) ;
#982 =( LENGTH_UNIT ( ) NAMED_UNIT ( * ) SI_UNIT ( .MILLI., .METRE. ) );
#983 = SURFACE_STYLE_USAGE ( .BOTH. , #720 ) ;
#984 = EDGE_LOOP ( 'NONE', ( #2241, #2447, #2019, #1978, #3024, #2576, #596, #895 ) ) ;
#985 = AXIS2_PLACEMENT_3D ( 'NONE', #1976, #2688, #2443 ) ;
#986 = CARTESIAN_POINT ( 'NONE',  ( 140.0000000000000000, -6.928842772166554697E-15, 7.500000000000000000 ) ) ;
#987 = COLOUR_RGB ( '',0.8941176470588234615, 0.8941176470588234615, 0.8941176470588234615 ) ;
#988 = DIRECTION ( 'NONE',  ( 1.000000000000000000, 0.000000000000000000, -0.000000000000000000 ) ) ;
#989 = EDGE_LOOP ( 'NONE', ( #2526, #57, #564, #96, #3116, #3195, #136, #1328 ) ) ;
#990 = EDGE_LOOP ( 'NONE', ( #2913, #1504 ) ) ;
#991 = CYLINDRICAL_SURFACE ( 'NONE', #652, 5.000000000000000000 ) ;
#992 = CARTESIAN_POINT ( 'NONE',  ( 36.60604563826976943, -1.460666791800804498, 16.38100777177576362 ) ) ;
#993 = FACE_OUTER_BOUND ( 'NONE', #854, .T. ) ;
#994 = ADVANCED_FACE ( 'NONE', ( #1911 ), #1579, .T. ) ;
#995 = ITEM_DEFINED_TRANSFORMATION ( 'NONE', 'NONE', #1591,  #2878 ) ;
#996 = CARTESIAN_POINT ( 'NONE',  ( 3.033375984251970081, -8.673617379884035472E-16, 0.000000000000000000 ) ) ;
#997 = DIRECTION ( 'NONE',  ( 0.000000000000000000, 0.000000000000000000, 1.000000000000000000 ) ) ;
#998 =( NAMED_UNIT ( * ) SI_UNIT ( $, .STERADIAN. ) SOLID_ANGLE_UNIT ( ) );
#999 = ORIENTED_EDGE ( 'NONE', *, *, #2679, .F. ) ;
#1000 = AXIS2_PLACEMENT_3D ( 'NONE', #672, #1412, #2437 ) ;
#1001 = AXIS2_PLACEMENT_3D ( 'NONE', #791, #1545, #2988 ) ;
#1002 = CARTESIAN_POINT ( 'NONE',  ( 35.86950496355626683, 0.9908260551213666778, 16.44556929574713777 ) ) ;
#1003 = VECTOR ( 'NONE', #1553, 1000.000000000000000 ) ;
#1004 = SURFACE_STYLE_FILL_AREA ( #2890 ) ;
#1005 = DIRECTION ( 'NONE',  ( -0.000000000000000000, -0.000000000000000000, 1.000000000000000000 ) ) ;
#1006 = EDGE_CURVE ( 'NONE', #2037, #1232, #2098, .T. ) ;
#1007 = LINE ( 'NONE', #2488, #424 ) ;
#1008 = VECTOR ( 'NONE', #351, 1000.000000000000114 ) ;
#1009 = CIRCLE ( 'NONE', #2315, 14.00000000000000000 ) ;
#1010 =( GEOMETRIC_REPRESENTATION_CONTEXT ( 3 ) GLOBAL_UNCERTAINTY_ASSIGNED_CONTEXT ( ( #2860 ) ) GLOBAL_UNIT_ASSIGNED_CONTEXT ( ( #2794, #2764, #1312 ) ) REPRESENTATION_CONTEXT ( 'NONE', 'WORKASPACE' ) );
#1011 = EDGE_LOOP ( 'NONE', ( #607, #1544, #1039, #1313 ) ) ;
#1012 = ORIENTED_EDGE ( 'NONE', *, *, #772, .T. ) ;
#1013 = CARTESIAN_POINT ( 'NONE',  ( 1.617350269189632428, 0.000000000000000000, 0.000000000000000000 ) ) ;
#1014 = PLANE ( 'NONE',  #890 ) ;
#1015 = CARTESIAN_POINT ( 'NONE',  ( 37.41786025882474576, -7.616137346557303354E-15, 12.50000000000000000 ) ) ;
#1016 = DIRECTION ( 'NONE',  ( -0.000000000000000000, 0.000000000000000000, -1.000000000000000000 ) ) ;
#1017 =( NAMED_UNIT ( * ) SI_UNIT ( $, .STERADIAN. ) SOLID_ANGLE_UNIT ( ) );
#1018 = ORIENTED_EDGE ( 'NONE', *, *, #866, .F. ) ;
#1019 = CARTESIAN_POINT ( 'NONE',  ( 0.000000000000000000, 0.000000000000000000, 2.849999999999999645 ) ) ;
#1020 = CARTESIAN_POINT ( 'NONE',  ( -23.99999999999999645, -6.928842772166554697E-15, 7.500000000000000000 ) ) ;
#1021 = AXIS2_PLACEMENT_3D ( 'NONE', #1457, #2451, #218 ) ;
#1022 = ADVANCED_FACE ( 'NONE', ( #171 ), #221, .T. ) ;
#1023 = VERTEX_POINT ( 'NONE', #2929 ) ;
#1024 = CIRCLE ( 'NONE', #358, 5.000000000000000000 ) ;
#1025 = ORIENTED_EDGE ( 'NONE', *, *, #465, .T. ) ;
#1026 = EDGE_CURVE ( 'NONE', #3069, #2935, #1939, .T. ) ;
#1027 = CARTESIAN_POINT ( 'NONE',  ( 35.69898883018242230, -0.7529305858385405559, 16.46882038169669471 ) ) ;
#1028 = DIRECTION ( 'NONE',  ( 1.000000000000000000, 0.000000000000000000, 0.000000000000000000 ) ) ;
#1029 = CARTESIAN_POINT ( 'NONE',  ( 140.0000000000000000, -6.928842772166554697E-15, 7.500000000000000000 ) ) ;
#1030 = VERTEX_POINT ( 'NONE', #1461 ) ;
#1031 = CONICAL_SURFACE ( 'NONE', #613, 4.999999999999998224, 1.029744258676654312 ) ;
#1032 = CARTESIAN_POINT ( 'NONE',  ( 38.50000000000000000, 1.474514954580286030E-14, 13.99999999999999822 ) ) ;
#1033 = ORIENTED_EDGE ( 'NONE', *, *, #2418, .F. ) ;
#1034 = ADVANCED_FACE ( 'NONE', ( #3206 ), #2711, .F. ) ;
#1035 = DIRECTION ( 'NONE',  ( -1.000000000000000000, 0.000000000000000000, 0.000000000000000000 ) ) ;
#1036 = PRESENTATION_STYLE_ASSIGNMENT (( #1283 ) ) ;
#1037 = FACE_OUTER_BOUND ( 'NONE', #875, .T. ) ;
#1038 = AXIS2_PLACEMENT_3D ( 'NONE', #2152, #1475, #2436 ) ;
#1039 = ORIENTED_EDGE ( 'NONE', *, *, #1721, .T. ) ;
#1040 = CARTESIAN_POINT ( 'NONE',  ( -26.99999999999999645, -7.622732162557277534E-15, 7.500000000000000000 ) ) ;
#1041 = CARTESIAN_POINT ( 'NONE',  ( 36.08479696852054985, -1.192462354422064497, 16.42082098627955844 ) ) ;
#1042 = FACE_OUTER_BOUND ( 'NONE', #885, .T. ) ;
#1043 = ORIENTED_EDGE ( 'NONE', *, *, #257, .T. ) ;
#1044 = EDGE_CURVE ( 'NONE', #1890, #79, #1895, .T. ) ;
#1045 = ADVANCED_FACE ( 'NONE', ( #2749 ), #744, .F. ) ;
#1046 = AXIS2_PLACEMENT_3D ( 'NONE', #2529, #2745, #266 ) ;
#1047 = DIRECTION ( 'NONE',  ( 1.000000000000000000, -0.000000000000000000, -0.000000000000000000 ) ) ;
#1048 = DIRECTION ( 'NONE',  ( -1.000000000000000000, -2.312964634635742957E-16, 0.000000000000000000 ) ) ;
#1049 = EDGE_LOOP ( 'NONE', ( #11, #3163, #2385, #847, #2923, #379 ) ) ;
#1050 = ADVANCED_BREP_SHAPE_REPRESENTATION ( '', ( #2136, #2878 ), #491 ) ;
#1051 = DIRECTION ( 'NONE',  ( -2.478176394252581634E-16, 1.000000000000000000, 0.000000000000000000 ) ) ;
#1052 = FACE_OUTER_BOUND ( 'NONE', #1325, .T. ) ;
#1053 = PRESENTATION_LAYER_ASSIGNMENT (  '', '', ( #489 ) ) ;
#1054 = MANIFOLD_SOLID_BREP ( 'Boss-Extrude1', #699 ) ;
#1055 = DIRECTION ( 'NONE',  ( -1.000000000000000000, -2.312964634635742957E-16, 0.000000000000000000 ) ) ;
#1056 = ORIENTED_EDGE ( 'NONE', *, *, #1551, .T. ) ;
#1057 = VECTOR ( 'NONE', #306, 1000.000000000000000 ) ;
#1058 = ORIENTED_EDGE ( 'NONE', *, *, #76, .F. ) ;
#1059 = AXIS2_PLACEMENT_3D ( 'NONE', #2007, #2907, #1933 ) ;
#1060 = AXIS2_PLACEMENT_3D ( 'NONE', #1040, #1830, #804 ) ;
#1061 = EDGE_CURVE ( 'NONE', #1916, #1595, #898, .T. ) ;
#1062 = CARTESIAN_POINT ( 'NONE',  ( 36.24410157368014751, -1.310477515365985557, 16.40440676504733730 ) ) ;
#1063 = CARTESIAN_POINT ( 'NONE',  ( 7.369500000000001272, 1.836970198721029934E-16, -1.500000000000000000 ) ) ;
#1064 = EDGE_LOOP ( 'NONE', ( #2176, #3018 ) ) ;
#1065 = PRESENTATION_LAYER_ASSIGNMENT (  '', '', ( #2111 ) ) ;
#1066 = DIRECTION ( 'NONE',  ( 1.000000000000000000, 0.000000000000000000, 0.000000000000000000 ) ) ;
#1067 = EDGE_CURVE ( 'NONE', #2004, #2636, #3079, .T. ) ;
#1068 = DIRECTION ( 'NONE',  ( 0.000000000000000000, 1.000000000000000000, 0.000000000000000000 ) ) ;
#1069 = ORIENTED_EDGE ( 'NONE', *, *, #1430, .F. ) ;
#1070 = ADVANCED_FACE ( 'NONE', ( #505, #1762 ), #1495, .F. ) ;
#1071 = CARTESIAN_POINT ( 'NONE',  ( 36.80294994545206322, 1.490236770648136089, 16.37578575999040353 ) ) ;
#1072 = ORIENTED_EDGE ( 'NONE', *, *, #7, .T. ) ;
#1073 = CARTESIAN_POINT ( 'NONE',  ( 36.80294994545205611, -1.490236770648107001, 16.37578575999040353 ) ) ;
#1074 = CIRCLE ( 'NONE', #2330, 2.849999999999999645 ) ;
#1075 = DIRECTION ( 'NONE',  ( 0.000000000000000000, 0.000000000000000000, -1.000000000000000000 ) ) ;
#1076 = VERTEX_POINT ( 'NONE', #2035 ) ;
#1077 = LINE ( 'NONE', #612, #2159 ) ;
#1078 = CARTESIAN_POINT ( 'NONE',  ( 1.750000000000000000, 1.959434878635764737E-16, -1.599999999999999645 ) ) ;
#1079 = EDGE_LOOP ( 'NONE', ( #933, #177, #3058, #1169 ) ) ;
#1080 = EDGE_CURVE ( 'NONE', #2998, #1599, #2718, .T. ) ;
#1081 = FACE_OUTER_BOUND ( 'NONE', #114, .T. ) ;
#1082 =( NAMED_UNIT ( * ) PLANE_ANGLE_UNIT ( ) SI_UNIT ( $, .RADIAN. ) );
#1083 = PRESENTATION_STYLE_ASSIGNMENT (( #1287 ) ) ;
#1084 = VERTEX_POINT ( 'NONE', #556 ) ;
#1085 = EDGE_CURVE ( 'NONE', #1226, #415, #20, .T. ) ;
#1086 = VECTOR ( 'NONE', #3210, 1000.000000000000000 ) ;
#1087 = CARTESIAN_POINT ( 'NONE',  ( 30.00000000000000000, 3.673940397442057600E-15, 0.000000000000000000 ) ) ;
#1088 = EDGE_CURVE ( 'NONE', #1709, #1829, #32, .T. ) ;
#1089 = DIRECTION ( 'NONE',  ( 0.000000000000000000, 0.000000000000000000, -1.000000000000000000 ) ) ;
#1090 = ORIENTED_EDGE ( 'NONE', *, *, #2497, .T. ) ;
#1091 = CARTESIAN_POINT ( 'NONE',  ( -23.99999999999999645, -6.928842772166554697E-15, 7.500000000000000000 ) ) ;
#1092 = EDGE_CURVE ( 'NONE', #3031, #417, #864, .T. ) ;
#1093 = CARTESIAN_POINT ( 'NONE',  ( 1.649999999999999911, 0.000000000000000000, 0.000000000000000000 ) ) ;
#1094 = CIRCLE ( 'NONE', #161, 8.999999999999992895 ) ;
#1095 = ORIENTED_EDGE ( 'NONE', *, *, #2970, .F. ) ;
#1096 = EDGE_LOOP ( 'NONE', ( #1090, #855, #1208, #2383, #406, #2169 ) ) ;
#1097 = DIRECTION ( 'NONE',  ( 1.000000000000000000, 0.000000000000000000, 0.000000000000000000 ) ) ;
#1098 = PRESENTATION_STYLE_ASSIGNMENT (( #2876 ) ) ;
#1099 = CONICAL_SURFACE ( 'NONE', #2559, 1.250000000000001110, 1.029744258676654090 ) ;
#1100 = EDGE_CURVE ( 'NONE', #2974, #2689, #1442, .T. ) ;
#1101 = DIRECTION ( 'NONE',  ( 0.000000000000000000, 0.000000000000000000, -1.000000000000000000 ) ) ;
#1102 = EDGE_LOOP ( 'NONE', ( #1025, #1417, #2065, #3212 ) ) ;
#1103 = CIRCLE ( 'NONE', #2209, 5.000000000000000000 ) ;
#1104 = EDGE_CURVE ( 'NONE', #108, #1246, #2532, .T. ) ;
#1105 = VECTOR ( 'NONE', #1744, 1000.000000000000000 ) ;
#1106 = ORIENTED_EDGE ( 'NONE', *, *, #1172, .F. ) ;
#1107 = CARTESIAN_POINT ( 'NONE',  ( 3.469446951953614189E-15, -15.00000000000000355, 15.00000000000000000 ) ) ;
#1108 = VERTEX_POINT ( 'NONE', #291 ) ;
#1109 = PRODUCT_DEFINITION_SHAPE ( 'NONE', 'NONE',  #3094 ) ;
#1110 = CARTESIAN_POINT ( 'NONE',  ( 47.00000000000000000, 14.00000000000001243, 7.500000000000000000 ) ) ;
#1111 = CIRCLE ( 'NONE', #1320, 10.00000000000000178 ) ;
#1112 = VECTOR ( 'NONE', #2342, 1000.000000000000000 ) ;
#1113 = STYLED_ITEM ( 'NONE', ( #1098 ), #1362 ) ;
#1114 = CYLINDRICAL_SURFACE ( 'NONE', #1861, 1.250000000000001110 ) ;
#1115 = COLOUR_RGB ( '',0.8941176470588234615, 0.8941176470588234615, 0.8941176470588234615 ) ;
#1116 = SHAPE_REPRESENTATION ( 'anvil', ( #2878 ), #2622 ) ;
#1117 = APPLICATION_PROTOCOL_DEFINITION ( 'draft international standard', 'automotive_design', 1998, #969 ) ;
#1118 = ORIENTED_EDGE ( 'NONE', *, *, #927, .F. ) ;
#1119 = VERTEX_POINT ( 'NONE', #1032 ) ;
#1120 = CARTESIAN_POINT ( 'NONE',  ( 140.0000000000000000, -6.928842772166554697E-15, 7.500000000000000000 ) ) ;
#1121 = ORIENTED_EDGE ( 'NONE', *, *, #192, .F. ) ;
#1122 = CARTESIAN_POINT ( 'NONE',  ( -37.00000000000000000, -5.000000000000010658, 7.500000000000000000 ) ) ;
#1123 = FACE_OUTER_BOUND ( 'NONE', #428, .T. ) ;
#1124 = ORIENTED_EDGE ( 'NONE', *, *, #1408, .F. ) ;
#1125 = UNCERTAINTY_MEASURE_WITH_UNIT (LENGTH_MEASURE( 1.000000000000000082E-05 ), #348, 'distance_accuracy_value', 'NONE');
#1126 = CARTESIAN_POINT ( 'NONE',  ( 4.336808689942017736E-16, 0.000000000000000000, 0.000000000000000000 ) ) ;
#1127 = EDGE_CURVE ( 'NONE', #3031, #1482, #792, .T. ) ;
#1128 = VERTEX_POINT ( 'NONE', #2544 ) ;
#1129 = DIRECTION ( 'NONE',  ( 1.000000000000000000, 0.000000000000000000, 0.000000000000000000 ) ) ;
#1130 = ORIENTED_EDGE ( 'NONE', *, *, #104, .T. ) ;
#1131 = CARTESIAN_POINT ( 'NONE',  ( 70.00000000000032685, -5.459266613189731341E-15, 19.50000000000000000 ) ) ;
#1132 = VECTOR ( 'NONE', #1607, 1000.000000000000000 ) ;
#1133 = CARTESIAN_POINT ( 'NONE',  ( 27.00000000000000000, 6.704247063196759979E-15, 7.500000000000000000 ) ) ;
#1134 = VERTEX_POINT ( 'NONE', #2295 ) ;
#1135 = ORIENTED_EDGE ( 'NONE', *, *, #1085, .T. ) ;
#1136 = DIRECTION ( 'NONE',  ( 0.000000000000000000, 0.000000000000000000, 1.000000000000000000 ) ) ;
#1137 = DIRECTION ( 'NONE',  ( 0.000000000000000000, 0.000000000000000000, -1.000000000000000000 ) ) ;
#1138 = FILL_AREA_STYLE_COLOUR ( '', #1115 ) ;
#1139 = ADVANCED_BREP_SHAPE_REPRESENTATION ( '', ( #2105, #2878 ), #1375 ) ;
#1140 = DIRECTION ( 'NONE',  ( -0.000000000000000000, 0.000000000000000000, -1.000000000000000000 ) ) ;
#1141 = ORIENTED_EDGE ( 'NONE', *, *, #76, .T. ) ;
#1142 = FACE_OUTER_BOUND ( 'NONE', #1994, .T. ) ;
#1143 = ORIENTED_EDGE ( 'NONE', *, *, #1149, .T. ) ;
#1144 = DIRECTION ( 'NONE',  ( -0.000000000000000000, -0.000000000000000000, -1.000000000000000000 ) ) ;
#1145 = ORIENTED_EDGE ( 'NONE', *, *, #1361, .F. ) ;
#1146 = CARTESIAN_POINT ( 'NONE',  ( -26.99999999999999645, -7.622732162557277534E-15, 7.500000000000000000 ) ) ;
#1147 = AXIS2_PLACEMENT_3D ( 'NONE', #374, #153, #2286 ) ;
#1148 = CARTESIAN_POINT ( 'NONE',  ( 27.00000000000000355, -13.99999999999999467, 7.500000000000001776 ) ) ;
#1149 = EDGE_CURVE ( 'NONE', #310, #2118, #512, .T. ) ;
#1150 = APPLICATION_PROTOCOL_DEFINITION ( 'draft international standard', 'automotive_design', 1998, #3199 ) ;
#1151 = CIRCLE ( 'NONE', #1985, 2.849999999999999645 ) ;
#1152 = EDGE_LOOP ( 'NONE', ( #2145, #412, #1160, #2143 ) ) ;
#1153 = CARTESIAN_POINT ( 'NONE',  ( 1.269999999999999796, 0.000000000000000000, 0.000000000000000000 ) ) ;
#1154 = CARTESIAN_POINT ( 'NONE',  ( 1.040000000000000036, 0.5773502691896263972, -1.000000000000000000 ) ) ;
#1155 = CYLINDRICAL_SURFACE ( 'NONE', #1262, 8.999999999999994671 ) ;
#1156 = ORIENTED_EDGE ( 'NONE', *, *, #2976, .T. ) ;
#1157 = DIRECTION ( 'NONE',  ( 0.000000000000000000, 0.000000000000000000, -1.000000000000000000 ) ) ;
#1158 = ORIENTED_EDGE ( 'NONE', *, *, #2761, .T. ) ;
#1159 = FACE_BOUND ( 'NONE', #624, .T. ) ;
#1160 = ORIENTED_EDGE ( 'NONE', *, *, #2742, .T. ) ;
#1161 = AXIS2_PLACEMENT_3D ( 'NONE', #1671, #2404, #2221 ) ;
#1162 = DIRECTION ( 'NONE',  ( -1.000000000000000000, -0.000000000000000000, -0.000000000000000000 ) ) ;
#1163 = CIRCLE ( 'NONE', #280, 12.00000000000000000 ) ;
#1164 = CARTESIAN_POINT ( 'NONE',  ( 27.00000000000000000, -7.622732162557277534E-15, 7.500000000000000000 ) ) ;
#1165 = CARTESIAN_POINT ( 'NONE',  ( 26.99999999999999645, 14.00000000000000711, 7.500000000000000000 ) ) ;
#1166 = DIRECTION ( 'NONE',  ( 1.000000000000000000, 0.000000000000000000, 0.000000000000000000 ) ) ;
#1167 = CIRCLE ( 'NONE', #592, 9.000000000000000000 ) ;
#1168 = CIRCLE ( 'NONE', #2674, 0.1000000000000000472 ) ;
#1169 = ORIENTED_EDGE ( 'NONE', *, *, #657, .F. ) ;
#1170 = CIRCLE ( 'NONE', #906, 1.500000000000001332 ) ;
#1171 = DIRECTION ( 'NONE',  ( 0.000000000000000000, 0.000000000000000000, -1.000000000000000000 ) ) ;
#1172 = EDGE_CURVE ( 'NONE', #1877, #877, #3057, .T. ) ;
#1173 = CARTESIAN_POINT ( 'NONE',  ( 70.00000000000032685, -6.928842772166554697E-15, -4.500000000000000888 ) ) ;
#1174 = ADVANCED_FACE ( 'NONE', ( #3082 ), #1649, .T. ) ;
#1175 = MECHANICAL_DESIGN_GEOMETRIC_PRESENTATION_REPRESENTATION (  '', ( #2677 ), #3200 ) ;
#1176 = EDGE_CURVE ( 'NONE', #1134, #1570, #1853, .T. ) ;
#1177 = DIRECTION ( 'NONE',  ( 0.000000000000000000, 0.000000000000000000, 1.000000000000000000 ) ) ;
#1178 = VERTEX_POINT ( 'NONE', #2337 ) ;
#1179 = CARTESIAN_POINT ( 'NONE',  ( 35.80050950286611311, 0.9216565616594220023, 16.45376772233409923 ) ) ;
#1180 = ORIENTED_EDGE ( 'NONE', *, *, #1661, .F. ) ;
#1181 = DIRECTION ( 'NONE',  ( -1.000000000000000000, -0.000000000000000000, -0.000000000000000000 ) ) ;
#1182 = VERTEX_POINT ( 'NONE', #2837 ) ;
#1183 = FACE_OUTER_BOUND ( 'NONE', #2367, .T. ) ;
#1184 = DIRECTION ( 'NONE',  ( 1.000000000000000000, 2.312964634635742957E-16, 0.000000000000000000 ) ) ;
#1185 = DIRECTION ( 'NONE',  ( 0.000000000000000000, 0.000000000000000000, 1.000000000000000000 ) ) ;
#1186 = DIRECTION ( 'NONE',  ( -1.000000000000000000, -0.000000000000000000, -0.000000000000000000 ) ) ;
#1187 = CARTESIAN_POINT ( 'NONE',  ( -29.99999999999999645, -15.00000000000000355, 0.000000000000000000 ) ) ;
#1188 = CIRCLE ( 'NONE', #2903, 5.000000000000000000 ) ;
#1189 = EDGE_CURVE ( 'NONE', #2624, #2847, #1600, .T. ) ;
#1190 = PRODUCT_DEFINITION_CONTEXT ( 'detailed design', #808, 'design' ) ;
#1191 = CARTESIAN_POINT ( 'NONE',  ( 1.040000000000000036, 1.154700538379252350, -1.084202172485497162E-16 ) ) ;
#1192 = EDGE_CURVE ( 'NONE', #2397, #2430, #193, .T. ) ;
#1193 = CARTESIAN_POINT ( 'NONE',  ( 36.60604563826974811, 1.460666791800832254, 16.38100777177577072 ) ) ;
#1194 = ORIENTED_EDGE ( 'NONE', *, *, #2761, .F. ) ;
#1195 = DIRECTION ( 'NONE',  ( -1.000000000000000000, -2.312964634635743450E-16, -0.000000000000000000 ) ) ;
#1196 = EDGE_LOOP ( 'NONE', ( #3078, #2672 ) ) ;
#1197 = LINE ( 'NONE', #2196, #2973 ) ;
#1198 = DIRECTION ( 'NONE',  ( 1.000000000000000000, 2.312964634635742957E-16, 0.000000000000000000 ) ) ;
#1199 = DIRECTION ( 'NONE',  ( 1.000000000000000000, -0.000000000000000000, -0.000000000000000000 ) ) ;
#1200 = CONTEXT_DEPENDENT_SHAPE_REPRESENTATION ( #311, #2390 ) ;
#1201 = CARTESIAN_POINT ( 'NONE',  ( 47.00000000000000000, 1.133017633246824530E-14, 7.500000000000000000 ) ) ;
#1202 = AXIS2_PLACEMENT_3D ( 'NONE', #1630, #2958, #1171 ) ;
#1203 = CYLINDRICAL_SURFACE ( 'NONE', #284, 5.000000000000000888 ) ;
#1204 = CONICAL_SURFACE ( 'NONE', #377, 1732.050807568857181, 1.047197551196592746 ) ;
#1205 = CARTESIAN_POINT ( 'NONE',  ( 1.040000000000000036, 0.8660254037844390407, -0.5000000000000002220 ) ) ;
#1206 = EDGE_CURVE ( 'NONE', #658, #2850, #2177, .T. ) ;
#1207 = ORIENTED_EDGE ( 'NONE', *, *, #2422, .T. ) ;
#1208 = ORIENTED_EDGE ( 'NONE', *, *, #761, .T. ) ;
#1209 = FACE_OUTER_BOUND ( 'NONE', #1575, .T. ) ;
#1210 = CARTESIAN_POINT ( 'NONE',  ( 100.0000000000000000, -6.928842772166554697E-15, 7.500000000000000000 ) ) ;
#1211 = CARTESIAN_POINT ( 'NONE',  ( 1.040000000000000036, -1.154700538379251684, -1.199226976249124676E-17 ) ) ;
#1212 = CARTESIAN_POINT ( 'NONE',  ( -30.00000000000000000, -8.316621552948000372E-15, 15.00000000000000000 ) ) ;
#1213 = VECTOR ( 'NONE', #394, 1000.000000000000114 ) ;
#1214 =( LENGTH_UNIT ( ) NAMED_UNIT ( * ) SI_UNIT ( .MILLI., .METRE. ) );
#1215 = AXIS2_PLACEMENT_3D ( 'NONE', #1827, #1332, #1802 ) ;
#1216 = LINE ( 'NONE', #2947, #3135 ) ;
#1217 = FILL_AREA_STYLE ('',( #1245 ) ) ;
#1218 = CIRCLE ( 'NONE', #2724, 1.000000000000000000 ) ;
#1219 = CIRCLE ( 'NONE', #2885, 8.000000000000000000 ) ;
#1220 = PRESENTATION_LAYER_ASSIGNMENT (  '', '', ( #1899 ) ) ;
#1221 = PLANE ( 'NONE',  #647 ) ;
#1222 = PRESENTATION_LAYER_ASSIGNMENT (  '', '', ( #1650 ) ) ;
#1223 = CARTESIAN_POINT ( 'NONE',  ( 1.040000000000000036, 0.5773502691896263972, -1.000000000000000000 ) ) ;
#1224 = CYLINDRICAL_SURFACE ( 'NONE', #1680, 5.000000000000000888 ) ;
#1225 = ORIENTED_EDGE ( 'NONE', *, *, #2062, .T. ) ;
#1226 = VERTEX_POINT ( 'NONE', #1354 ) ;
#1227 = EDGE_CURVE ( 'NONE', #391, #628, #923, .T. ) ;
#1228 = CARTESIAN_POINT ( 'NONE',  ( 37.39427925860091051, -1.460378464396907328, 16.38104908776753632 ) ) ;
#1229 = LINE ( 'NONE', #2968, #1309 ) ;
#1230 = CARTESIAN_POINT ( 'NONE',  ( 37.10670076043889765, -0.3922264638554286975, 12.48459209977295181 ) ) ;
#1231 = CARTESIAN_POINT ( 'NONE',  ( 1.040000000000000036, 0.000000000000000000, 0.000000000000000000 ) ) ;
#1232 = VERTEX_POINT ( 'NONE', #2371 ) ;
#1233 = VECTOR ( 'NONE', #2894, 1000.000000000000000 ) ;
#1234 = ADVANCED_FACE ( 'NONE', ( #851 ), #1114, .F. ) ;
#1235 = DIRECTION ( 'NONE',  ( 0.000000000000000000, 0.000000000000000000, -1.000000000000000000 ) ) ;
#1236 = CARTESIAN_POINT ( 'NONE',  ( 3.469446951953614189E-15, -15.00000000000000355, 0.000000000000000000 ) ) ;
#1237 = ORIENTED_EDGE ( 'NONE', *, *, #295, .T. ) ;
#1238 = EDGE_LOOP ( 'NONE', ( #1589, #1095 ) ) ;
#1239 = CARTESIAN_POINT ( 'NONE',  ( -41.99999999999999289, 7.499999999999988454, 7.500000000000000888 ) ) ;
#1240 = LINE ( 'NONE', #2986, #1735 ) ;
#1241 = CARTESIAN_POINT ( 'NONE',  ( 1.040000000000000036, -1.154700538379251684, 0.000000000000000000 ) ) ;
#1242 = DIRECTION ( 'NONE',  ( 0.000000000000000000, 0.000000000000000000, 1.000000000000000000 ) ) ;
#1243 = EDGE_CURVE ( 'NONE', #745, #488, #2809, .T. ) ;
#1244 =( NAMED_UNIT ( * ) PLANE_ANGLE_UNIT ( ) SI_UNIT ( $, .RADIAN. ) );
#1245 = FILL_AREA_STYLE_COLOUR ( '', #809 ) ;
#1246 = VERTEX_POINT ( 'NONE', #3067 ) ;
#1247 = AXIS2_PLACEMENT_3D ( 'NONE', #3011, #1055, #2024 ) ;
#1248 = CARTESIAN_POINT ( 'NONE',  ( 38.12949724085409997, 0.9918543271721460552, 16.44544909559322932 ) ) ;
#1249 = CARTESIAN_POINT ( 'NONE',  ( -26.99999999999999645, 7.499999999999992006, 7.500000000000000888 ) ) ;
#1250 = PRESENTATION_LAYER_ASSIGNMENT (  '', '', ( #1410 ) ) ;
#1251 = DIRECTION ( 'NONE',  ( -1.000000000000000000, -0.000000000000000000, -0.000000000000000000 ) ) ;
#1252 = ORIENTED_EDGE ( 'NONE', *, *, #2595, .T. ) ;
#1253 = EDGE_LOOP ( 'NONE', ( #1918, #1934, #2174, #320 ) ) ;
#1254 = DIRECTION ( 'NONE',  ( 1.000000000000000000, 2.312964634635743450E-16, 0.000000000000000000 ) ) ;
#1255 = CARTESIAN_POINT ( 'NONE',  ( 36.80088933932602657, -1.499879510127380522, 16.37414004115126431 ) ) ;
#1256 = DIRECTION ( 'NONE',  ( -1.000000000000000000, -0.000000000000000000, -0.000000000000000000 ) ) ;
#1257 = CARTESIAN_POINT ( 'NONE',  ( 37.00000000000000000, 1.474514954580286030E-14, 20.99999999999999645 ) ) ;
#1258 = AXIS2_PLACEMENT_3D ( 'NONE', #2990, #522, #762 ) ;
#1259 = UNCERTAINTY_MEASURE_WITH_UNIT (LENGTH_MEASURE( 1.000000000000000082E-05 ), #2994, 'distance_accuracy_value', 'NONE');
#1260 = CARTESIAN_POINT ( 'NONE',  ( -37.00000000000000000, -5.785761963836251101E-15, 7.500000000000000000 ) ) ;
#1261 = ORIENTED_EDGE ( 'NONE', *, *, #1734, .T. ) ;
#1262 = AXIS2_PLACEMENT_3D ( 'NONE', #2618, #2901, #659 ) ;
#1263 = ADVANCED_FACE ( 'NONE', ( #387 ), #405, .T. ) ;
#1264 = PRODUCT_DEFINITION ( 'UNKNOWN', '', #1910, #290 ) ;
#1265 = AXIS2_PLACEMENT_3D ( 'NONE', #368, #80, #3066 ) ;
#1266 = DIRECTION ( 'NONE',  ( -1.000000000000000000, -0.000000000000000000, -0.000000000000000000 ) ) ;
#1267 = AXIS2_PLACEMENT_3D ( 'NONE', #1382, #2155, #1101 ) ;
#1268 = CARTESIAN_POINT ( 'NONE',  ( 1.040000000000000036, 0.000000000000000000, 0.000000000000000000 ) ) ;
#1269 = DIRECTION ( 'NONE',  ( 0.000000000000000000, 0.000000000000000000, -1.000000000000000000 ) ) ;
#1270 = AXIS2_PLACEMENT_3D ( 'NONE', #78, #1129, #644 ) ;
#1271 = AXIS2_PLACEMENT_3D ( 'NONE', #23, #2252, #4 ) ;
#1272 = FILL_AREA_STYLE_COLOUR ( '', #2054 ) ;
#1273 = ORIENTED_EDGE ( 'NONE', *, *, #2997, .T. ) ;
#1274 = CARTESIAN_POINT ( 'NONE',  ( 7.369500000000001272, 0.000000000000000000, 1.499999999999999778 ) ) ;
#1275 = DIRECTION ( 'NONE',  ( 0.000000000000000000, 0.000000000000000000, -1.000000000000000000 ) ) ;
#1276 = DIRECTION ( 'NONE',  ( 0.000000000000000000, 1.000000000000000000, 0.000000000000000000 ) ) ;
#1277 = CARTESIAN_POINT ( 'NONE',  ( -26.99999999999999645, -5.785761963836251101E-15, 7.500000000000000000 ) ) ;
#1278 = PRESENTATION_STYLE_ASSIGNMENT (( #2763 ) ) ;
#1279 = ORIENTED_EDGE ( 'NONE', *, *, #667, .T. ) ;
#1280 = ORIENTED_EDGE ( 'NONE', *, *, #329, .F. ) ;
#1281 = CARTESIAN_POINT ( 'NONE',  ( -23.99999999999999645, -5.000000000000007994, 7.500000000000000000 ) ) ;
#1282 = ADVANCED_FACE ( 'NONE', ( #2116 ), #583, .T. ) ;
#1283 = SURFACE_STYLE_USAGE ( .BOTH. , #1597 ) ;
#1284 = CARTESIAN_POINT ( 'NONE',  ( 140.0000000000000000, -6.928842772166554697E-15, 7.500000000000000000 ) ) ;
#1285 = AXIS2_PLACEMENT_3D ( 'NONE', #1078, #369, #1822 ) ;
#1286 = EDGE_CURVE ( 'NONE', #2092, #1779, #1374, .T. ) ;
#1287 = SURFACE_STYLE_USAGE ( .BOTH. , #2768 ) ;
#1288 = CIRCLE ( 'NONE', #2072, 1.250000000000001110 ) ;
#1289 = ORIENTED_EDGE ( 'NONE', *, *, #2593, .T. ) ;
#1290 = CARTESIAN_POINT ( 'NONE',  ( 30.00000000000000355, -15.00000000000000355, 0.000000000000000000 ) ) ;
#1291 = DIRECTION ( 'NONE',  ( 0.000000000000000000, 0.000000000000000000, -1.000000000000000000 ) ) ;
#1292 = CARTESIAN_POINT ( 'NONE',  ( -26.99999999999999645, -5.173438564262573782E-15, 12.49999999999999822 ) ) ;
#1293 = EDGE_LOOP ( 'NONE', ( #2363, #69, #2551, #840 ) ) ;
#1294 = DIRECTION ( 'NONE',  ( 0.000000000000000000, 0.000000000000000000, -1.000000000000000000 ) ) ;
#1295 = DIRECTION ( 'NONE',  ( 1.000000000000000000, 2.312964634635743450E-16, 0.000000000000000000 ) ) ;
#1296 =( NAMED_UNIT ( * ) PLANE_ANGLE_UNIT ( ) SI_UNIT ( $, .RADIAN. ) );
#1297 = ORIENTED_EDGE ( 'NONE', *, *, #2619, .F. ) ;
#1298 = DIRECTION ( 'NONE',  ( 1.000000000000000000, 0.000000000000000000, 0.000000000000000000 ) ) ;
#1299 = DIRECTION ( 'NONE',  ( 1.000000000000000000, 0.000000000000000000, 0.000000000000000000 ) ) ;
#1300 = CIRCLE ( 'NONE', #263, 8.000000000000000000 ) ;
#1301 = CARTESIAN_POINT ( 'NONE',  ( 3.033375984251970081, -8.673617379884035472E-16, 0.000000000000000000 ) ) ;
#1302 = ORIENTED_EDGE ( 'NONE', *, *, #3048, .F. ) ;
#1303 = EDGE_CURVE ( 'NONE', #2965, #1482, #1593, .T. ) ;
#1304 = CARTESIAN_POINT ( 'NONE',  ( -5.000000000000000000, -6.928842772166554697E-15, 2.499999999999999556 ) ) ;
#1305 = CARTESIAN_POINT ( 'NONE',  ( 1.750000000000000000, 1.836970198721029441E-16, -1.499999999999999556 ) ) ;
#1306 = LINE ( 'NONE', #319, #1921 ) ;
#1307 = ORIENTED_EDGE ( 'NONE', *, *, #3093, .T. ) ;
#1308 = EDGE_CURVE ( 'NONE', #1904, #3197, #2853, .T. ) ;
#1309 = VECTOR ( 'NONE', #1439, 1000.000000000000000 ) ;
#1310 = DIRECTION ( 'NONE',  ( 1.000000000000000000, 0.000000000000000000, 0.000000000000000000 ) ) ;
#1311 = FILL_AREA_STYLE_COLOUR ( '', #697 ) ;
#1312 =( NAMED_UNIT ( * ) SI_UNIT ( $, .STERADIAN. ) SOLID_ANGLE_UNIT ( ) );
#1313 = ORIENTED_EDGE ( 'NONE', *, *, #1688, .F. ) ;
#1314 = CARTESIAN_POINT ( 'NONE',  ( 37.39427925860091051, 1.460378464396937304, 16.38104908776753277 ) ) ;
#1315 =( NAMED_UNIT ( * ) PLANE_ANGLE_UNIT ( ) SI_UNIT ( $, .RADIAN. ) );
#1316 = VECTOR ( 'NONE', #271, 1000.000000000000000 ) ;
#1317 = AXIS2_PLACEMENT_3D ( 'NONE', #2581, #2862, #2829 ) ;
#1318 = PRESENTATION_LAYER_ASSIGNMENT (  '', '', ( #2723 ) ) ;
#1319 = ORIENTED_EDGE ( 'NONE', *, *, #298, .F. ) ;
#1320 = AXIS2_PLACEMENT_3D ( 'NONE', #878, #2334, #1388 ) ;
#1321 =( GEOMETRIC_REPRESENTATION_CONTEXT ( 3 ) GLOBAL_UNCERTAINTY_ASSIGNED_CONTEXT ( ( #1687 ) ) GLOBAL_UNIT_ASSIGNED_CONTEXT ( ( #425, #1615, #1633 ) ) REPRESENTATION_CONTEXT ( 'NONE', 'WORKASPACE' ) );
#1322 = CARTESIAN_POINT ( 'NONE',  ( 35.57671993710910385, -0.4836543419624433349, 16.48745487577124180 ) ) ;
#1323 = DIRECTION ( 'NONE',  ( 0.000000000000000000, 0.000000000000000000, 1.000000000000000000 ) ) ;
#1324 = ADVANCED_FACE ( 'NONE', ( #355 ), #134, .T. ) ;
#1325 = EDGE_LOOP ( 'NONE', ( #859, #2531, #1528, #2705, #1558, #97 ) ) ;
#1326 = DIRECTION ( 'NONE',  ( -1.000000000000000000, -2.312964634635742957E-16, 0.000000000000000000 ) ) ;
#1327 = DIRECTION ( 'NONE',  ( -1.000000000000000000, -0.000000000000000000, -0.000000000000000000 ) ) ;
#1328 = ORIENTED_EDGE ( 'NONE', *, *, #1821, .F. ) ;
#1329 = EDGE_CURVE ( 'NONE', #1182, #2676, #1667, .T. ) ;
#1330 = FACE_OUTER_BOUND ( 'NONE', #2812, .T. ) ;
#1331 = ADVANCED_FACE ( 'NONE', ( #2709 ), #140, .F. ) ;
#1332 = DIRECTION ( 'NONE',  ( 1.000000000000000000, 0.000000000000000000, 0.000000000000000000 ) ) ;
#1333 = EDGE_LOOP ( 'NONE', ( #619, #1611, #2598, #83 ) ) ;
#1334 = AXIS2_PLACEMENT_3D ( 'NONE', #1407, #2697, #2401 ) ;
#1335 = EDGE_CURVE ( 'NONE', #2821, #576, #668, .T. ) ;
#1336 = CARTESIAN_POINT ( 'NONE',  ( 36.90254329834229452, -1.500037116461185871, 16.37411340082286770 ) ) ;
#1337 = VECTOR ( 'NONE', #554, 1000.000000000000000 ) ;
#1338 = CARTESIAN_POINT ( 'NONE',  ( 37.10600482971271674, 0.3921370382570182889, 12.48459913632445506 ) ) ;
#1339 = EDGE_LOOP ( 'NONE', ( #905, #3083 ) ) ;
#1340 = FACE_OUTER_BOUND ( 'NONE', #1064, .T. ) ;
#1341 = DIRECTION ( 'NONE',  ( -1.000000000000000000, -0.000000000000000000, -0.000000000000000000 ) ) ;
#1342 = VERTEX_POINT ( 'NONE', #150 ) ;
#1343 = ORIENTED_EDGE ( 'NONE', *, *, #1408, .T. ) ;
#1344 = APPLICATION_CONTEXT ( 'automotive_design' ) ;
#1345 = ADVANCED_FACE ( 'NONE', ( #2387 ), #971, .F. ) ;
#1346 = CARTESIAN_POINT ( 'NONE',  ( 0.000000000000000000, -0.5773502691896253980, -1.000000000000000000 ) ) ;
#1347 = DIRECTION ( 'NONE',  ( -1.000000000000000000, -0.000000000000000000, -0.000000000000000000 ) ) ;
#1348 = DIRECTION ( 'NONE',  ( -2.312964634635742957E-16, 1.000000000000000000, 0.000000000000000000 ) ) ;
#1349 = ORIENTED_EDGE ( 'NONE', *, *, #2110, .T. ) ;
#1350 = DIRECTION ( 'NONE',  ( 0.8571673007021121116, 0.000000000000000000, 0.5150380749100544886 ) ) ;
#1351 = CARTESIAN_POINT ( 'NONE',  ( 38.49999999999999289, 1.474514954580286030E-14, 16.49999999999999289 ) ) ;
#1352 = ORIENTED_EDGE ( 'NONE', *, *, #44, .F. ) ;
#1353 = CARTESIAN_POINT ( 'NONE',  ( 1.040000000000000036, -0.5773502691896253980, -1.000000000000000000 ) ) ;
#1354 = CARTESIAN_POINT ( 'NONE',  ( 100.0000000000000000, -6.928842772166554697E-15, 16.50000000000000000 ) ) ;
#1355 = CARTESIAN_POINT ( 'NONE',  ( 0.000000000000000000, 0.000000000000000000, 0.000000000000000000 ) ) ;
#1356 = AXIS2_PLACEMENT_3D ( 'NONE', #1456, #202, #1936 ) ;
#1357 = ORIENTED_EDGE ( 'NONE', *, *, #2924, .T. ) ;
#1358 = ORIENTED_EDGE ( 'NONE', *, *, #1080, .T. ) ;
#1359 = DIRECTION ( 'NONE',  ( -2.312964634635742957E-16, 1.000000000000000000, 0.000000000000000000 ) ) ;
#1360 = CARTESIAN_POINT ( 'NONE',  ( 41.99999999999999289, 1.017369401515037180E-14, 7.500000000000000000 ) ) ;
#1361 = EDGE_CURVE ( 'NONE', #1849, #1023, #2235, .T. ) ;
#1362 = ADVANCED_BREP_SHAPE_REPRESENTATION ( '', ( #2099, #2878 ), #2622 ) ;
#1363 = AXIS2_PLACEMENT_3D ( 'NONE', #2734, #2249, #1546 ) ;
#1364 = DIRECTION ( 'NONE',  ( 0.000000000000000000, 1.000000000000000000, 0.000000000000000000 ) ) ;
#1365 = VERTEX_POINT ( 'NONE', #1148 ) ;
#1366 = DIRECTION ( 'NONE',  ( 0.000000000000000000, 0.000000000000000000, -1.000000000000000000 ) ) ;
#1367 = AXIS2_PLACEMENT_3D ( 'NONE', #928, #1397, #1140 ) ;
#1368 = AXIS2_PLACEMENT_3D ( 'NONE', #1909, #2016, #2777 ) ;
#1369 = EDGE_LOOP ( 'NONE', ( #2626, #1872, #2293, #364 ) ) ;
#1370 = CARTESIAN_POINT ( 'NONE',  ( 1.040000000000000036, -1.154700538379251684, -1.199226976249124676E-17 ) ) ;
#1371 = ORIENTED_EDGE ( 'NONE', *, *, #1686, .F. ) ;
#1372 = DIRECTION ( 'NONE',  ( 0.000000000000000000, 0.000000000000000000, -1.000000000000000000 ) ) ;
#1373 = AXIS2_PLACEMENT_3D ( 'NONE', #765, #2227, #265 ) ;
#1374 = LINE ( 'NONE', #2067, #2691 ) ;
#1375 =( GEOMETRIC_REPRESENTATION_CONTEXT ( 3 ) GLOBAL_UNCERTAINTY_ASSIGNED_CONTEXT ( ( #1894 ) ) GLOBAL_UNIT_ASSIGNED_CONTEXT ( ( #557, #584, #1017 ) ) REPRESENTATION_CONTEXT ( 'NONE', 'WORKASPACE' ) );
#1376 = DIRECTION ( 'NONE',  ( 1.000000000000000000, 0.000000000000000000, 0.000000000000000000 ) ) ;
#1377 = ORIENTED_EDGE ( 'NONE', *, *, #1797, .T. ) ;
#1378 = ORIENTED_EDGE ( 'NONE', *, *, #1127, .T. ) ;
#1379 = CARTESIAN_POINT ( 'NONE',  ( 35.50000000000000000, 1.243235838461289750E-14, 16.49999999999999289 ) ) ;
#1380 = DIRECTION ( 'NONE',  ( 1.000000000000000000, 0.000000000000000000, 0.000000000000000000 ) ) ;
#1381 = DIRECTION ( 'NONE',  ( 0.000000000000000000, 0.000000000000000000, 1.000000000000000000 ) ) ;
#1382 = CARTESIAN_POINT ( 'NONE',  ( -5.000000000000000000, -6.928842772166554697E-15, 7.500000000000000000 ) ) ;
#1383 = ORIENTED_EDGE ( 'NONE', *, *, #2382, .T. ) ;
#1384 = CARTESIAN_POINT ( 'NONE',  ( 1.040000000000000036, -1.154700538379251684, 0.000000000000000000 ) ) ;
#1385 = EDGE_CURVE ( 'NONE', #1916, #2721, #1937, .T. ) ;
#1386 = ADVANCED_FACE ( 'NONE', ( #2199 ), #1426, .T. ) ;
#1387 = ORIENTED_EDGE ( 'NONE', *, *, #1361, .T. ) ;
#1388 = DIRECTION ( 'NONE',  ( 0.000000000000000000, 0.000000000000000000, -1.000000000000000000 ) ) ;
#1389 = ORIENTED_EDGE ( 'NONE', *, *, #2656, .F. ) ;
#1390 = CARTESIAN_POINT ( 'NONE',  ( 35.75000000000000000, 1.489823039569627924E-14, 20.99999999999999645 ) ) ;
#1391 = CARTESIAN_POINT ( 'NONE',  ( 100.0000000000000000, -6.928842772166554697E-15, 7.500000000000000000 ) ) ;
#1392 =( NAMED_UNIT ( * ) PLANE_ANGLE_UNIT ( ) SI_UNIT ( $, .RADIAN. ) );
#1393 = VERTEX_POINT ( 'NONE', #2927 ) ;
#1394 = FACE_OUTER_BOUND ( 'NONE', #2795, .T. ) ;
#1395 = DIRECTION ( 'NONE',  ( 1.000000000000000000, 0.000000000000000000, 0.000000000000000000 ) ) ;
#1396 = PRESENTATION_STYLE_ASSIGNMENT (( #156 ) ) ;
#1397 = DIRECTION ( 'NONE',  ( 1.000000000000000000, 0.000000000000000000, -0.000000000000000000 ) ) ;
#1398 = ORIENTED_EDGE ( 'NONE', *, *, #1308, .F. ) ;
#1399 = CARTESIAN_POINT ( 'NONE',  ( 36.24736826332971162, 1.301195037071590122, 16.40561087244777028 ) ) ;
#1400 = ORIENTED_EDGE ( 'NONE', *, *, #510, .T. ) ;
#1401 = LINE ( 'NONE', #3147, #2161 ) ;
#1402 = ORIENTED_EDGE ( 'NONE', *, *, #3037, .F. ) ;
#1403 = EDGE_CURVE ( 'NONE', #163, #1964, #2183, .T. ) ;
#1404 = DIRECTION ( 'NONE',  ( -1.000000000000000000, -0.000000000000000000, -0.000000000000000000 ) ) ;
#1405 = CIRCLE ( 'NONE', #2651, 30.00000000000000000 ) ;
#1406 = PRODUCT_RELATED_PRODUCT_CATEGORY ( 'part', '', ( #1647 ) ) ;
#1408 = EDGE_CURVE ( 'NONE', #640, #2397, #2167, .T. ) ;
#1407 = CARTESIAN_POINT ( 'NONE',  ( 4.336808689942017736E-16, 0.000000000000000000, 0.000000000000000000 ) ) ;
#1409 = APPLICATION_PROTOCOL_DEFINITION ( 'draft international standard', 'automotive_design', 1998, #1850 ) ;
#1410=STYLED_ITEM('',(#3236),#2136);
#1411 = ORIENTED_EDGE ( 'NONE', *, *, #1303, .F. ) ;
#1412 = DIRECTION ( 'NONE',  ( -1.000000000000000000, -0.000000000000000000, -0.000000000000000000 ) ) ;
#1413 =( LENGTH_UNIT ( ) NAMED_UNIT ( * ) SI_UNIT ( .MILLI., .METRE. ) );
#1414 = CARTESIAN_POINT ( 'NONE',  ( 1.040000000000000036, 1.154700538379252350, -1.084202172485497162E-16 ) ) ;
#1415 = VERTEX_POINT ( 'NONE', #2644 ) ;
#1416 = CARTESIAN_POINT ( 'NONE',  ( 35.53942839536622955, 0.3936020622859700002, 16.49320894598176679 ) ) ;
#1417 = ORIENTED_EDGE ( 'NONE', *, *, #1026, .T. ) ;
#1418 = DIRECTION ( 'NONE',  ( 0.000000000000000000, -1.000000000000000000, 0.000000000000000000 ) ) ;
#1419 = EDGE_LOOP ( 'NONE', ( #142, #1925, #1642, #1594 ) ) ;
#1420 =( GEOMETRIC_REPRESENTATION_CONTEXT ( 3 ) GLOBAL_UNCERTAINTY_ASSIGNED_CONTEXT ( ( #3107 ) ) GLOBAL_UNIT_ASSIGNED_CONTEXT ( ( #982, #1244, #2001 ) ) REPRESENTATION_CONTEXT ( 'NONE', 'WORKASPACE' ) );
#1421 = LINE ( 'NONE', #3201, #956 ) ;
#1422 = PRODUCT_DEFINITION_CONTEXT ( 'detailed design', #133, 'design' ) ;
#1423 = AXIS2_PLACEMENT_3D ( 'NONE', #2115, #65, #3098 ) ;
#1424 = EDGE_CURVE ( 'NONE', #1595, #2776, #3151, .T. ) ;
#1425 = LINE ( 'NONE', #1681, #326 ) ;
#1426 = CYLINDRICAL_SURFACE ( 'NONE', #817, 8.999999999999994671 ) ;
#1427 =( GEOMETRIC_REPRESENTATION_CONTEXT ( 3 ) GLOBAL_UNCERTAINTY_ASSIGNED_CONTEXT ( ( #2498 ) ) GLOBAL_UNIT_ASSIGNED_CONTEXT ( ( #1452, #1664, #3164 ) ) REPRESENTATION_CONTEXT ( 'NONE', 'WORKASPACE' ) );
#1428 = CIRCLE ( 'NONE', #1060, 7.500000000000000000 ) ;
#1429 = CARTESIAN_POINT ( 'NONE',  ( 87.00000000000000000, -7.622732162557277534E-15, 16.49999999999999289 ) ) ;
#1430 = EDGE_CURVE ( 'NONE', #1779, #877, #1715, .T. ) ;
#1431 = CARTESIAN_POINT ( 'NONE',  ( 155.0000000000000284, -6.316519372592878167E-15, 2.499999999999999556 ) ) ;
#1432 = CYLINDRICAL_SURFACE ( 'NONE', #2465, 30.00000000000000000 ) ;
#1433 = EDGE_CURVE ( 'NONE', #1023, #1694, #1609, .T. ) ;
#1434 = DIRECTION ( 'NONE',  ( -1.000000000000000000, 0.000000000000000000, -0.000000000000000000 ) ) ;
#1435 = ORIENTED_EDGE ( 'NONE', *, *, #1508, .F. ) ;
#1436 = LINE ( 'NONE', #1693, #2002 ) ;
#1437 = ORIENTED_EDGE ( 'NONE', *, *, #2633, .F. ) ;
#1438 = CARTESIAN_POINT ( 'NONE',  ( 1.040000000000000036, -1.154700538379251684, -1.199226976249124676E-17 ) ) ;
#1439 = DIRECTION ( 'NONE',  ( -2.312964634635742957E-16, 1.000000000000000000, 0.000000000000000000 ) ) ;
#1440 = CARTESIAN_POINT ( 'NONE',  ( 47.00000000000000000, 1.243235845170086321E-14, 16.49999999999999289 ) ) ;
#1441 = SURFACE_STYLE_FILL_AREA ( #1926 ) ;
#1442 = CIRCLE ( 'NONE', #3158, 5.000000000000000000 ) ;
#1443 = CARTESIAN_POINT ( 'NONE',  ( 30.00000000000000000, 3.673940397442057600E-15, 15.00000000000000000 ) ) ;
#1444 = SHAPE_REPRESENTATION_RELATIONSHIP ( 'NONE' , 'NONE' ,  #1790, #2267 ) ;
#1445 = AXIS2_PLACEMENT_3D ( 'NONE', #304, #2774, #2511 ) ;
#1446 = EDGE_CURVE ( 'NONE', #2348, #745, #622, .T. ) ;
#1447 = UNCERTAINTY_MEASURE_WITH_UNIT (LENGTH_MEASURE( 1.000000000000000082E-05 ), #2588, 'distance_accuracy_value', 'NONE');
#1448 = DIRECTION ( 'NONE',  ( -1.000000000000000000, -0.000000000000000000, -0.000000000000000000 ) ) ;
#1449 = ADVANCED_FACE ( 'NONE', ( #966 ), #1031, .F. ) ;
#1450 = CARTESIAN_POINT ( 'NONE',  ( 150.0000000000000000, -6.928842772166554697E-15, 2.499999999999999556 ) ) ;
#1451 = EDGE_LOOP ( 'NONE', ( #2053, #464, #1357, #2567, #2755, #687 ) ) ;
#1452 =( LENGTH_UNIT ( ) NAMED_UNIT ( * ) SI_UNIT ( .MILLI., .METRE. ) );
#1453 = ORIENTED_EDGE ( 'NONE', *, *, #811, .T. ) ;
#1454 = FACE_BOUND ( 'NONE', #2335, .T. ) ;
#1455 = CARTESIAN_POINT ( 'NONE',  ( 7.369500000000001272, 0.000000000000000000, 0.000000000000000000 ) ) ;
#1456 = CARTESIAN_POINT ( 'NONE',  ( 1.750000000000000000, 0.000000000000000000, 0.000000000000000000 ) ) ;
#1457 = CARTESIAN_POINT ( 'NONE',  ( 3.469446951953614189E-15, -15.00000000000000355, 0.000000000000000000 ) ) ;
#1458 = APPLICATION_PROTOCOL_DEFINITION ( 'draft international standard', 'automotive_design', 1998, #2741 ) ;
#1459 = AXIS2_PLACEMENT_3D ( 'NONE', #1800, #2389, #1891 ) ;
#1460 = DIRECTION ( 'NONE',  ( 0.000000000000000000, 0.000000000000000000, 1.000000000000000000 ) ) ;
#1461 = CARTESIAN_POINT ( 'NONE',  ( 27.00000000000000000, -7.622732162557275957E-15, 16.49999999999999289 ) ) ;
#1462 = FILL_AREA_STYLE_COLOUR ( '', #910 ) ;
#1463 = EDGE_CURVE ( 'NONE', #2676, #1182, #2899, .T. ) ;
#1464 = FACE_OUTER_BOUND ( 'NONE', #1152, .T. ) ;
#1465 = VECTOR ( 'NONE', #214, 1000.000000000000000 ) ;
#1466 = DIRECTION ( 'NONE',  ( 1.000000000000000000, 2.312964634635742957E-16, 0.000000000000000000 ) ) ;
#1467 = EDGE_LOOP ( 'NONE', ( #3062, #1889 ) ) ;
#1468 = EDGE_LOOP ( 'NONE', ( #2834, #2398, #1884, #1349, #283 ) ) ;
#1469 = CARTESIAN_POINT ( 'NONE',  ( 41.99999999999999289, 1.017369401515037180E-14, 7.500000000000000000 ) ) ;
#1470 = CARTESIAN_POINT ( 'NONE',  ( 37.75516277711825808, -1.310683246666488833, 16.40437238582925872 ) ) ;
#1471 = FACE_OUTER_BOUND ( 'NONE', #1079, .T. ) ;
#1472 = CARTESIAN_POINT ( 'NONE',  ( 155.0000000000000284, -6.928842772166554697E-15, 15.50000000000000000 ) ) ;
#1473 = CIRCLE ( 'NONE', #2154, 5.000000000000000000 ) ;
#1474 = ITEM_DEFINED_TRANSFORMATION ( 'NONE', 'NONE', #70,  #2878 ) ;
#1475 = DIRECTION ( 'NONE',  ( 1.000000000000000000, -0.000000000000000000, -0.000000000000000000 ) ) ;
#1476 = EDGE_CURVE ( 'NONE', #877, #1503, #2429, .T. ) ;
#1477 = AXIS2_PLACEMENT_3D ( 'NONE', #1301, #588, #2073 ) ;
#1478 = LINE ( 'NONE', #1431, #3191 ) ;
#1479 =( LENGTH_UNIT ( ) NAMED_UNIT ( * ) SI_UNIT ( .MILLI., .METRE. ) );
#1480 = MECHANICAL_DESIGN_GEOMETRIC_PRESENTATION_REPRESENTATION (  '', ( #2108 ), #1427 ) ;
#1481 = AXIS2_PLACEMENT_3D ( 'NONE', #3076, #1846, #2772 ) ;
#1482 = VERTEX_POINT ( 'NONE', #1212 ) ;
#1483 = EDGE_CURVE ( 'NONE', #1595, #1916, #1188, .T. ) ;
#1484 = DIRECTION ( 'NONE',  ( 1.000000000000000000, 0.000000000000000000, 0.000000000000000000 ) ) ;
#1485 = AXIS2_PLACEMENT_3D ( 'NONE', #649, #632, #1166 ) ;
#1486 = PLANE ( 'NONE',  #2395 ) ;
#1487 = AXIS2_PLACEMENT_3D ( 'NONE', #889, #1381, #2377 ) ;
#1488 = EDGE_LOOP ( 'NONE', ( #868, #2266, #709, #2653 ) ) ;
#1489 = VERTEX_POINT ( 'NONE', #2957 ) ;
#1490 = EDGE_CURVE ( 'NONE', #640, #1128, #515, .T. ) ;
#1491 = CARTESIAN_POINT ( 'NONE',  ( 1.269999999999999796, 3.490243377569956061E-16, -2.849999999999999645 ) ) ;
#1492 = CARTESIAN_POINT ( 'NONE',  ( 140.0000000000000000, -5.949125332848671934E-15, -0.5000000000000004441 ) ) ;
#1493 = CARTESIAN_POINT ( 'NONE',  ( 36.78831377322251228, -0.3533019008417399021, 12.48801788595628892 ) ) ;
#1494 = DIRECTION ( 'NONE',  ( 1.000000000000000000, -0.000000000000000000, -0.000000000000000000 ) ) ;
#1495 = PLANE ( 'NONE',  #2507 ) ;
#1496 =( LENGTH_UNIT ( ) NAMED_UNIT ( * ) SI_UNIT ( .MILLI., .METRE. ) );
#1497 = ORIENTED_EDGE ( 'NONE', *, *, #2340, .T. ) ;
#1498 = AXIS2_PLACEMENT_3D ( 'NONE', #2352, #1341, #2870 ) ;
#1499 = CIRCLE ( 'NONE', #84, 5.000000000000000888 ) ;
#1500 = DIRECTION ( 'NONE',  ( -0.8571673007021121116, 1.049727191138618449E-16, 0.5150380749100544886 ) ) ;
#1501 = DIRECTION ( 'NONE',  ( -1.000000000000000000, -0.000000000000000000, -0.000000000000000000 ) ) ;
#1502 = CARTESIAN_POINT ( 'NONE',  ( 1.040000000000000036, -1.154700538379251684, 0.000000000000000000 ) ) ;
#1503 = VERTEX_POINT ( 'NONE', #1729 ) ;
#1504 = ORIENTED_EDGE ( 'NONE', *, *, #2742, .F. ) ;
#1505 = DIRECTION ( 'NONE',  ( -1.000000000000000000, -0.000000000000000000, -0.000000000000000000 ) ) ;
#1506 = LINE ( 'NONE', #2244, #2550 ) ;
#1507 = CARTESIAN_POINT ( 'NONE',  ( 38.25000000000000000, 1.474514954580286030E-14, 13.99999999999999822 ) ) ;
#1508 = EDGE_CURVE ( 'NONE', #1709, #779, #1543, .T. ) ;
#1509 =( NAMED_UNIT ( * ) PLANE_ANGLE_UNIT ( ) SI_UNIT ( $, .RADIAN. ) );
#1510 = EDGE_CURVE ( 'NONE', #241, #1621, #1288, .T. ) ;
#1511 = DIRECTION ( 'NONE',  ( -1.000000000000000000, -2.312964634635742957E-16, 0.000000000000000000 ) ) ;
#1512 = EDGE_LOOP ( 'NONE', ( #833, #1770, #1669 ) ) ;
#1513 = AXIS2_PLACEMENT_3D ( 'NONE', #813, #3050, #138 ) ;
#1514 = CARTESIAN_POINT ( 'NONE',  ( 26.99999999999999645, 14.00000000000000711, 7.500000000000000000 ) ) ;
#1515 =( NAMED_UNIT ( * ) PLANE_ANGLE_UNIT ( ) SI_UNIT ( $, .RADIAN. ) );
#1516 = APPLICATION_CONTEXT ( 'automotive_design' ) ;
#1517 = CARTESIAN_POINT ( 'NONE',  ( 37.00000000000000000, 1.474514954580286030E-14, 13.99999999999999822 ) ) ;
#1518 = DIRECTION ( 'NONE',  ( 0.000000000000000000, 1.000000000000000000, 0.000000000000000000 ) ) ;
#1519 = CIRCLE ( 'NONE', #1356, 1.499999999999999556 ) ;
#1520 = ORIENTED_EDGE ( 'NONE', *, *, #2006, .T. ) ;
#1521 = LINE ( 'NONE', #216, #3141 ) ;
#1522 = FACE_OUTER_BOUND ( 'NONE', #2096, .T. ) ;
#1523 = FACE_BOUND ( 'NONE', #264, .T. ) ;
#1524 = DIRECTION ( 'NONE',  ( -1.000000000000000000, -0.000000000000000000, -0.000000000000000000 ) ) ;
#1525 = EDGE_CURVE ( 'NONE', #1604, #1342, #2031, .T. ) ;
#1526 = DIRECTION ( 'NONE',  ( 0.000000000000000000, 0.000000000000000000, -1.000000000000000000 ) ) ;
#1527 = SURFACE_SIDE_STYLE ('',( #1547 ) ) ;
#1528 = ORIENTED_EDGE ( 'NONE', *, *, #1176, .T. ) ;
#1529 = AXIS2_PLACEMENT_3D ( 'NONE', #1414, #175, #2173 ) ;
#1530 = ADVANCED_FACE ( 'NONE', ( #2728, #2969 ), #2530, .T. ) ;
#1531 = AXIS2_PLACEMENT_3D ( 'NONE', #1257, #1984, #2971 ) ;
#1532 = CARTESIAN_POINT ( 'NONE',  ( 36.51683924005257609, 1.423460261948054750, 16.38679996801885252 ) ) ;
#1533 =( LENGTH_UNIT ( ) NAMED_UNIT ( * ) SI_UNIT ( .MILLI., .METRE. ) );
#1534 = DIRECTION ( 'NONE',  ( 1.000000000000000000, -0.000000000000000000, -0.000000000000000000 ) ) ;
#1535 = AXIS2_PLACEMENT_3D ( 'NONE', #2789, #1291, #1818 ) ;
#1536 = AXIS2_PLACEMENT_3D ( 'NONE', #2756, #1713, #2013 ) ;
#1537 =( GEOMETRIC_REPRESENTATION_CONTEXT ( 3 ) GLOBAL_UNCERTAINTY_ASSIGNED_CONTEXT ( ( #2180 ) ) GLOBAL_UNIT_ASSIGNED_CONTEXT ( ( #1496, #1296, #793 ) ) REPRESENTATION_CONTEXT ( 'NONE', 'WORKASPACE' ) );
#1538 = ORIENTED_EDGE ( 'NONE', *, *, #839, .F. ) ;
#1539 = ORIENTED_EDGE ( 'NONE', *, *, #591, .F. ) ;
#1540 = PRODUCT_DEFINITION_FORMATION_WITH_SPECIFIED_SOURCE ( 'ANY', '', #2617, .NOT_KNOWN. ) ;
#1541 = CARTESIAN_POINT ( 'NONE',  ( 47.00000000000000000, 1.243235845170086321E-14, 16.49999999999998579 ) ) ;
#1542 = CARTESIAN_POINT ( 'NONE',  ( 36.24736826332972583, -1.301195037071565030, 16.40561087244777738 ) ) ;
#1543 = LINE ( 'NONE', #1292, #673 ) ;
#1544 = ORIENTED_EDGE ( 'NONE', *, *, #1656, .F. ) ;
#1545 = DIRECTION ( 'NONE',  ( -1.000000000000000000, -0.000000000000000000, -0.000000000000000000 ) ) ;
#1546 = DIRECTION ( 'NONE',  ( 0.000000000000000000, 1.000000000000000000, 0.000000000000000000 ) ) ;
#1547 = SURFACE_STYLE_FILL_AREA ( #2279 ) ;
#1548 = ORIENTED_EDGE ( 'NONE', *, *, #2033, .F. ) ;
#1549 = CARTESIAN_POINT ( 'NONE',  ( 38.19275052663392245, 0.9148478194932688767, 16.45375607287287423 ) ) ;
#1550 = DIRECTION ( 'NONE',  ( -2.478176394252581634E-16, 1.000000000000000000, 0.000000000000000000 ) ) ;
#1551 = EDGE_CURVE ( 'NONE', #1882, #87, #246, .T. ) ;
#1552 = DIRECTION ( 'NONE',  ( 0.000000000000000000, 0.000000000000000000, -1.000000000000000000 ) ) ;
#1553 = DIRECTION ( 'NONE',  ( -1.000000000000000000, -0.000000000000000000, -0.000000000000000000 ) ) ;
#1554 = ORIENTED_EDGE ( 'NONE', *, *, #329, .T. ) ;
#1555 = CARTESIAN_POINT ( 'NONE',  ( 37.00000000000000000, 1.474514954580286030E-14, 13.99999999999999822 ) ) ;
#1556 = CARTESIAN_POINT ( 'NONE',  ( 1.040000000000000036, -0.5773502691896253980, -1.000000000000000000 ) ) ;
#1557 = DIRECTION ( 'NONE',  ( -0.000000000000000000, -0.000000000000000000, 1.000000000000000000 ) ) ;
#1558 = ORIENTED_EDGE ( 'NONE', *, *, #3166, .F. ) ;
#1559 = DIRECTION ( 'NONE',  ( 0.000000000000000000, 0.000000000000000000, -1.000000000000000000 ) ) ;
#1560 = DIRECTION ( 'NONE',  ( 0.000000000000000000, -1.000000000000000000, 0.000000000000000000 ) ) ;
#1561 = VERTEX_POINT ( 'NONE', #3017 ) ;
#1562 = CARTESIAN_POINT ( 'NONE',  ( 0.000000000000000000, 1.154700538379252350, -1.084202172485497162E-16 ) ) ;
#1563 =( NAMED_UNIT ( * ) SI_UNIT ( $, .STERADIAN. ) SOLID_ANGLE_UNIT ( ) );
#1564 = ADVANCED_FACE ( 'NONE', ( #1042 ), #534, .F. ) ;
#1565 = EDGE_LOOP ( 'NONE', ( #2027, #1018, #3065, #1121 ) ) ;
#1566 =( GEOMETRIC_REPRESENTATION_CONTEXT ( 3 ) GLOBAL_UNCERTAINTY_ASSIGNED_CONTEXT ( ( #380 ) ) GLOBAL_UNIT_ASSIGNED_CONTEXT ( ( #1214, #1717, #2699 ) ) REPRESENTATION_CONTEXT ( 'NONE', 'WORKASPACE' ) );
#1567 = ORIENTED_EDGE ( 'NONE', *, *, #1127, .F. ) ;
#1568 = CYLINDRICAL_SURFACE ( 'NONE', #600, 14.00000000000000000 ) ;
#1569 = CARTESIAN_POINT ( 'NONE',  ( 140.0000000000000000, -6.928842772166554697E-15, 7.500000000000000000 ) ) ;
#1570 = VERTEX_POINT ( 'NONE', #1997 ) ;
#1571 = CIRCLE ( 'NONE', #2302, 10.00000000000000178 ) ;
#1572 = CARTESIAN_POINT ( 'NONE',  ( -30.00000000000000000, -8.316621552948000372E-15, 7.500000000000000000 ) ) ;
#1573 = DIRECTION ( 'NONE',  ( -0.000000000000000000, -0.000000000000000000, 1.000000000000000000 ) ) ;
#1574 = SURFACE_STYLE_USAGE ( .BOTH. , #2810 ) ;
#1575 = EDGE_LOOP ( 'NONE', ( #2542, #635, #651, #1398, #152 ) ) ;
#1576 = EDGE_CURVE ( 'NONE', #2721, #403, #618, .T. ) ;
#1577 = APPLICATION_CONTEXT ( 'automotive_design' ) ;
#1578 = FACE_OUTER_BOUND ( 'NONE', #1196, .T. ) ;
#1579 = CONICAL_SURFACE ( 'NONE', #1635, 12.00000000000000000, 0.09966865249115851311 ) ;
#1580 = EDGE_CURVE ( 'NONE', #3130, #466, #195, .T. ) ;
#1581 = AXIS2_PLACEMENT_3D ( 'NONE', #2731, #1524, #1242 ) ;
#1582 =( GEOMETRIC_REPRESENTATION_CONTEXT ( 3 ) GLOBAL_UNCERTAINTY_ASSIGNED_CONTEXT ( ( #1125 ) ) GLOBAL_UNIT_ASSIGNED_CONTEXT ( ( #348, #2288, #2041 ) ) REPRESENTATION_CONTEXT ( 'NONE', 'WORKASPACE' ) );
#1583 = DIRECTION ( 'NONE',  ( -0.000000000000000000, 0.000000000000000000, -1.000000000000000000 ) ) ;
#1584 = VECTOR ( 'NONE', #2573, 1000.000000000000114 ) ;
#1585 = ORIENTED_EDGE ( 'NONE', *, *, #1026, .F. ) ;
#1586 = VECTOR ( 'NONE', #2478, 1000.000000000000000 ) ;
#1587 = CARTESIAN_POINT ( 'NONE',  ( 36.51683924005256188, -1.423460261948026995, 16.38679996801885252 ) ) ;
#1588 = CARTESIAN_POINT ( 'NONE',  ( 36.78802102464440082, 0.3529434585571357696, 12.48803557435225287 ) ) ;
#1589 = ORIENTED_EDGE ( 'NONE', *, *, #1869, .F. ) ;
#1590 = ADVANCED_FACE ( 'NONE', ( #2046, #3035 ), #504, .T. ) ;
#1591 = AXIS2_PLACEMENT_3D ( 'NONE', #2645, #853, #867 ) ;
#1592 = LINE ( 'NONE', #1353, #1584 ) ;
#1593 = LINE ( 'NONE', #2323, #3059 ) ;
#1594 = ORIENTED_EDGE ( 'NONE', *, *, #252, .F. ) ;
#1595 = VERTEX_POINT ( 'NONE', #2790 ) ;
#1596 = CARTESIAN_POINT ( 'NONE',  ( -37.00000000000000000, 4.999999999999991118, 7.500000000000000888 ) ) ;
#1597 = SURFACE_SIDE_STYLE ('',( #542 ) ) ;
#1598 = PLANE ( 'NONE',  #490 ) ;
#1599 = VERTEX_POINT ( 'NONE', #978 ) ;
#1600 = CIRCLE ( 'NONE', #722, 1.250000000000001110 ) ;
#1601 = CARTESIAN_POINT ( 'NONE',  ( 35.49999999999999289, -0.09798730130380635395, 16.49999999999999645 ) ) ;
#1602 = AXIS2_PLACEMENT_3D ( 'NONE', #930, #2381, #1434 ) ;
#1603 = CARTESIAN_POINT ( 'NONE',  ( 100.0000000000000000, -6.928842772166554697E-15, 7.500000000000000000 ) ) ;
#1604 = VERTEX_POINT ( 'NONE', #1472 ) ;
#1605 = DIRECTION ( 'NONE',  ( -3.854941057726240069E-16, 1.000000000000000000, 0.000000000000000000 ) ) ;
#1606 = EDGE_CURVE ( 'NONE', #2776, #861, #3168, .T. ) ;
#1607 = DIRECTION ( 'NONE',  ( 1.000000000000000000, -0.000000000000000000, -0.000000000000000000 ) ) ;
#1608 = DIRECTION ( 'NONE',  ( 1.000000000000000000, 0.000000000000000000, 0.000000000000000000 ) ) ;
#1609 = CIRCLE ( 'NONE', #1334, 1.425000000000000044 ) ;
#1610 = ORIENTED_EDGE ( 'NONE', *, *, #2361, .T. ) ;
#1611 = ORIENTED_EDGE ( 'NONE', *, *, #2298, .T. ) ;
#1612 = DIRECTION ( 'NONE',  ( 0.000000000000000000, 0.000000000000000000, 1.000000000000000000 ) ) ;
#1613 = ADVANCED_FACE ( 'NONE', ( #1523, #993 ), #757, .F. ) ;
#1614 = PLANE ( 'NONE',  #224 ) ;
#1615 =( NAMED_UNIT ( * ) PLANE_ANGLE_UNIT ( ) SI_UNIT ( $, .RADIAN. ) );
#1616 = CARTESIAN_POINT ( 'NONE',  ( 60.00000000000000000, -6.928842772166554697E-15, -3.500000000000003109 ) ) ;
#1617 = ORIENTED_EDGE ( 'NONE', *, *, #2613, .T. ) ;
#1618 = CIRCLE ( 'NONE', #985, 8.000000000000000000 ) ;
#1619 = EDGE_CURVE ( 'NONE', #373, #401, #1074, .T. ) ;
#1620 = CARTESIAN_POINT ( 'NONE',  ( 37.91396272957889124, 1.193436492094938517, 16.42069107455876065 ) ) ;
#1621 = VERTEX_POINT ( 'NONE', #3003 ) ;
#1622 = CYLINDRICAL_SURFACE ( 'NONE', #2464, 8.000000000000000000 ) ;
#1623 = EDGE_LOOP ( 'NONE', ( #1352, #1652 ) ) ;
#1624 = CARTESIAN_POINT ( 'NONE',  ( 47.00000000000000000, 3.708099243547851920, 20.99999999999999645 ) ) ;
#1625 = DIRECTION ( 'NONE',  ( 1.000000000000000000, 0.000000000000000000, 0.000000000000000000 ) ) ;
#1626 = CARTESIAN_POINT ( 'NONE',  ( 0.000000000000000000, 0.000000000000000000, 0.000000000000000000 ) ) ;
#1627 = CIRCLE ( 'NONE', #1046, 14.00000000000000000 ) ;
#1628 = ORIENTED_EDGE ( 'NONE', *, *, #2308, .F. ) ;
#1629 = EDGE_LOOP ( 'NONE', ( #231, #1908, #1554, #1673 ) ) ;
#1630 = CARTESIAN_POINT ( 'NONE',  ( 47.00000000000000000, 1.133017633246824530E-14, 7.500000000000000000 ) ) ;
#1631 = DIRECTION ( 'NONE',  ( 0.000000000000000000, 1.000000000000000000, 0.000000000000000000 ) ) ;
#1632 = PRODUCT_DEFINITION_CONTEXT ( 'detailed design', #3199, 'design' ) ;
#1633 =( NAMED_UNIT ( * ) SI_UNIT ( $, .STERADIAN. ) SOLID_ANGLE_UNIT ( ) );
#1634 = EDGE_CURVE ( 'NONE', #770, #738, #1499, .T. ) ;
#1635 = AXIS2_PLACEMENT_3D ( 'NONE', #1719, #2700, #457 ) ;
#1636 = CARTESIAN_POINT ( 'NONE',  ( 47.00000000000000000, 1.133017633246824530E-14, 20.99999999999999645 ) ) ;
#1637 = ORIENTED_EDGE ( 'NONE', *, *, #2639, .F. ) ;
#1638 = FACE_OUTER_BOUND ( 'NONE', #125, .T. ) ;
#1639 = VECTOR ( 'NONE', #1876, 1000.000000000000000 ) ;
#1640 = AXIS2_PLACEMENT_3D ( 'NONE', #99, #72, #574 ) ;
#1641 = AXIS2_PLACEMENT_3D ( 'NONE', #1572, #1326, #2822 ) ;
#1642 = ORIENTED_EDGE ( 'NONE', *, *, #2970, .T. ) ;
#1643 = CARTESIAN_POINT ( 'NONE',  ( 36.63137859968045262, 0.2107904407421468673, 12.49606198580778660 ) ) ;
#1644 = AXIS2_PLACEMENT_3D ( 'NONE', #1902, #860, #2091 ) ;
#1645 = CIRCLE ( 'NONE', #1481, 4.999999999999998224 ) ;
#1646 = EDGE_LOOP ( 'NONE', ( #1389, #3044, #1676, #1069, #2280 ) ) ;
#1647 = PRODUCT ( 'Graduated Stationary Sleeve Barrel', 'Graduated Stationary Sleeve Barrel', '', ( #1938 ) ) ;
#1648 = DIRECTION ( 'NONE',  ( 1.000000000000000000, 0.000000000000000000, 0.000000000000000000 ) ) ;
#1649 = CYLINDRICAL_SURFACE ( 'NONE', #1498, 2.849999999999999645 ) ;
#1650 = STYLED_ITEM ( 'NONE', ( #1396 ), #3045 ) ;
#1651 =( NAMED_UNIT ( * ) PLANE_ANGLE_UNIT ( ) SI_UNIT ( $, .RADIAN. ) );
#1652 = ORIENTED_EDGE ( 'NONE', *, *, #1006, .F. ) ;
#1653 = DIRECTION ( 'NONE',  ( -1.000000000000000000, -0.000000000000000000, -0.000000000000000000 ) ) ;
#1654 = PRODUCT_DEFINITION_FORMATION_WITH_SPECIFIED_SOURCE ( 'ANY', '', #2716, .NOT_KNOWN. ) ;
#1655 = CARTESIAN_POINT ( 'NONE',  ( 150.0000000000000000, -6.928842772166554697E-15, 7.500000000000000000 ) ) ;
#1656 = EDGE_CURVE ( 'NONE', #1119, #531, #36, .T. ) ;
#1657 = CARTESIAN_POINT ( 'NONE',  ( 3.033375984251970081, -8.673617379884035472E-16, 0.000000000000000000 ) ) ;
#1658 = ORIENTED_EDGE ( 'NONE', *, *, #1100, .T. ) ;
#1659 = PRODUCT_DEFINITION ( 'UNKNOWN', '', #3090, #1632 ) ;
#1660 = FACE_BOUND ( 'NONE', #1725, .T. ) ;
#1661 = EDGE_CURVE ( 'NONE', #546, #2077, #1306, .T. ) ;
#1662 = ORIENTED_EDGE ( 'NONE', *, *, #2188, .T. ) ;
#1663 = ADVANCED_FACE ( 'NONE', ( #568 ), #2396, .F. ) ;
#1664 =( NAMED_UNIT ( * ) PLANE_ANGLE_UNIT ( ) SI_UNIT ( $, .RADIAN. ) );
#1665 = ORIENTED_EDGE ( 'NONE', *, *, #372, .F. ) ;
#1666 = DIRECTION ( 'NONE',  ( 0.000000000000000000, 0.000000000000000000, 1.000000000000000000 ) ) ;
#1667 = CIRCLE ( 'NONE', #201, 2.849999999999999645 ) ;
#1668 = DIRECTION ( 'NONE',  ( -1.000000000000000000, -0.000000000000000000, -0.000000000000000000 ) ) ;
#1669 = ORIENTED_EDGE ( 'NONE', *, *, #1088, .T. ) ;
#1670 = PRESENTATION_STYLE_ASSIGNMENT (( #670 ) ) ;
#1671 = CARTESIAN_POINT ( 'NONE',  ( 155.0000000000000284, -6.928842772166554697E-15, 7.500000000000000000 ) ) ;
#1672 = CARTESIAN_POINT ( 'NONE',  ( -37.00000000000000000, -9.935696797193021379E-15, 7.500000000000000000 ) ) ;
#1673 = ORIENTED_EDGE ( 'NONE', *, *, #1793, .F. ) ;
#1674 = DIRECTION ( 'NONE',  ( 1.000000000000000000, 0.000000000000000000, -0.000000000000000000 ) ) ;
#1675 = ADVANCED_FACE ( 'NONE', ( #1660, #3162 ), #2669, .F. ) ;
#1676 = ORIENTED_EDGE ( 'NONE', *, *, #1172, .T. ) ;
#1677 = FILL_AREA_STYLE ('',( #5 ) ) ;
#1678 = VERTEX_POINT ( 'NONE', #1880 ) ;
#1679 = CARTESIAN_POINT ( 'NONE',  ( 35.50000000000000711, 1.492884656567496302E-14, 20.99999999999999645 ) ) ;
#1680 = AXIS2_PLACEMENT_3D ( 'NONE', #1962, #2753, #2271 ) ;
#1681 = CARTESIAN_POINT ( 'NONE',  ( 38.25000000000000000, 1.474514954580286030E-14, 20.99999999999999645 ) ) ;
#1682 = CARTESIAN_POINT ( 'NONE',  ( 87.00000000000000000, -7.622732162557277534E-15, 7.500000000000000000 ) ) ;
#1683 =( NAMED_UNIT ( * ) SI_UNIT ( $, .STERADIAN. ) SOLID_ANGLE_UNIT ( ) );
#1684 = PLANE ( 'NONE',  #2665 ) ;
#1685 = CIRCLE ( 'NONE', #3025, 14.00000000000000000 ) ;
#1686 = EDGE_CURVE ( 'NONE', #2935, #1823, #1024, .T. ) ;
#1687 = UNCERTAINTY_MEASURE_WITH_UNIT (LENGTH_MEASURE( 1.000000000000000082E-05 ), #425, 'distance_accuracy_value', 'NONE');
#1688 = EDGE_CURVE ( 'NONE', #3100, #2088, #1848, .T. ) ;
#1689 = LINE ( 'NONE', #1249, #702 ) ;
#1690 = CARTESIAN_POINT ( 'NONE',  ( 37.48326775981566072, 1.423407605072616100, 16.38680797912481424 ) ) ;
#1691 =( REPRESENTATION_RELATIONSHIP ('NONE','NONE', #2426, #330 ) REPRESENTATION_RELATIONSHIP_WITH_TRANSFORMATION ( #1474 )SHAPE_REPRESENTATION_RELATIONSHIP( ) );
#1692 = ORIENTED_EDGE ( 'NONE', *, *, #677, .F. ) ;
#1693 = CARTESIAN_POINT ( 'NONE',  ( 52.00000000000000711, 3.708099243547853252, 20.99999999999999645 ) ) ;
#1694 = VERTEX_POINT ( 'NONE', #2904 ) ;
#1695 = VECTOR ( 'NONE', #2635, 1000.000000000000000 ) ;
#1696 = CARTESIAN_POINT ( 'NONE',  ( 140.0000000000000000, -6.928842772166554697E-15, 7.500000000000000000 ) ) ;
#1697 = AXIS2_PLACEMENT_3D ( 'NONE', #1091, #2586, #2836 ) ;
#1698 = VECTOR ( 'NONE', #1961, 1000.000000000000000 ) ;
#1699 = FACE_BOUND ( 'NONE', #1467, .T. ) ;
#1700 = DIRECTION ( 'NONE',  ( 0.000000000000000000, 0.000000000000000000, 1.000000000000000000 ) ) ;
#1701 = EDGE_CURVE ( 'NONE', #1756, #658, #926, .T. ) ;
#1702 = CIRCLE ( 'NONE', #2564, 13.00000000000000178 ) ;
#1703 = VECTOR ( 'NONE', #780, 1000.000000000000000 ) ;
#1704 = SURFACE_SIDE_STYLE ('',( #471 ) ) ;
#1705 = CARTESIAN_POINT ( 'NONE',  ( 1.040000000000000036, -1.154700538379251684, -1.199226976249124676E-17 ) ) ;
#1706 =( NAMED_UNIT ( * ) PLANE_ANGLE_UNIT ( ) SI_UNIT ( $, .RADIAN. ) );
#1707 = FACE_OUTER_BOUND ( 'NONE', #2787, .T. ) ;
#1708 = CARTESIAN_POINT ( 'NONE',  ( 47.00000000000000000, -3.708099243547826607, 20.99999999999999645 ) ) ;
#1709 = VERTEX_POINT ( 'NONE', #2175 ) ;
#1710 = FACE_OUTER_BOUND ( 'NONE', #1339, .T. ) ;
#1711 = EDGE_LOOP ( 'NONE', ( #643, #430, #2950, #332 ) ) ;
#1712 = FACE_OUTER_BOUND ( 'NONE', #2856, .T. ) ;
#1713 = DIRECTION ( 'NONE',  ( -1.000000000000000000, -0.000000000000000000, -0.000000000000000000 ) ) ;
#1714 = CARTESIAN_POINT ( 'NONE',  ( 30.00000000000000000, 3.673940397442057600E-15, 15.00000000000000000 ) ) ;
#1715 = LINE ( 'NONE', #1906, #1233 ) ;
#1716 = APPLICATION_PROTOCOL_DEFINITION ( 'draft international standard', 'automotive_design', 1998, #243 ) ;
#1717 =( NAMED_UNIT ( * ) PLANE_ANGLE_UNIT ( ) SI_UNIT ( $, .RADIAN. ) );
#1718 = ADVANCED_FACE ( 'NONE', ( #381, #1142 ), #1898, .F. ) ;
#1719 = CARTESIAN_POINT ( 'NONE',  ( 70.00000000000032685, -6.928842772166554697E-15, 7.500000000000000000 ) ) ;
#1720 = ADVANCED_FACE ( 'NONE', ( #1638 ), #2157, .T. ) ;
#1721 = EDGE_CURVE ( 'NONE', #1119, #2088, #913, .T. ) ;
#1722 = LINE ( 'NONE', #972, #549 ) ;
#1723 = FACE_BOUND ( 'NONE', #38, .T. ) ;
#1724 = ORIENTED_EDGE ( 'NONE', *, *, #1865, .T. ) ;
#1725 = EDGE_LOOP ( 'NONE', ( #3097, #1280 ) ) ;
#1726 = DIRECTION ( 'NONE',  ( 1.000000000000000000, 2.312964634635742957E-16, -0.000000000000000000 ) ) ;
#1727 = DIRECTION ( 'NONE',  ( 1.000000000000000000, 0.000000000000000000, 0.000000000000000000 ) ) ;
#1728 = CARTESIAN_POINT ( 'NONE',  ( 27.00000000000000000, -7.010408762983600216E-15, 2.499999999999999556 ) ) ;
#1729 = CARTESIAN_POINT ( 'NONE',  ( -41.99999999999999289, -15.00000000000000711, 0.000000000000000000 ) ) ;
#1730 = CIRCLE ( 'NONE', #95, 5.000000000000000000 ) ;
#1731 = DIRECTION ( 'NONE',  ( -1.000000000000000000, -0.000000000000000000, -0.000000000000000000 ) ) ;
#1732 = ORIENTED_EDGE ( 'NONE', *, *, #1812, .T. ) ;
#1733 = CARTESIAN_POINT ( 'NONE',  ( 1.040000000000000036, -0.5773502691896253980, -1.000000000000000000 ) ) ;
#1734 = EDGE_CURVE ( 'NONE', #1694, #1023, #1765, .T. ) ;
#1735 = VECTOR ( 'NONE', #519, 1000.000000000000227 ) ;
#1736 = CARTESIAN_POINT ( 'NONE',  ( 60.00000000000000000, -6.928842772166554697E-15, 7.500000000000000000 ) ) ;
#1737 = ORIENTED_EDGE ( 'NONE', *, *, #2864, .F. ) ;
#1738 = EDGE_LOOP ( 'NONE', ( #2568, #680, #1387, #3125, #49 ) ) ;
#1739 = PRODUCT_DEFINITION_SHAPE ( 'NONE', 'NONE',  #3224 ) ;
#1740 = FACE_OUTER_BOUND ( 'NONE', #665, .T. ) ;
#1741 = DIRECTION ( 'NONE',  ( 1.000000000000000000, 2.312964634635742957E-16, -0.000000000000000000 ) ) ;
#1742 = DIRECTION ( 'NONE',  ( 1.000000000000000000, -0.000000000000000000, -0.000000000000000000 ) ) ;
#1743 = AXIS2_PLACEMENT_3D ( 'NONE', #1875, #837, #1097 ) ;
#1744 = DIRECTION ( 'NONE',  ( -0.000000000000000000, -0.000000000000000000, 1.000000000000000000 ) ) ;
#1745 = CIRCLE ( 'NONE', #1840, 5.000000000000000000 ) ;
#1746 = AXIS2_PLACEMENT_3D ( 'NONE', #92, #2079, #2557 ) ;
#1747 = CIRCLE ( 'NONE', #66, 30.00000000000000000 ) ;
#1748 = VECTOR ( 'NONE', #1750, 1000.000000000000000 ) ;
#1749 = EDGE_LOOP ( 'NONE', ( #663, #675, #737, #1763 ) ) ;
#1750 = DIRECTION ( 'NONE',  ( -1.000000000000000000, -0.000000000000000000, -0.000000000000000000 ) ) ;
#1751 = AXIS2_PLACEMENT_3D ( 'NONE', #920, #2912, #1924 ) ;
#1752 = CARTESIAN_POINT ( 'NONE',  ( 155.0000000000000284, -6.928842772166554697E-15, 7.500000000000000000 ) ) ;
#1753 = EDGE_CURVE ( 'NONE', #1678, #87, #3126, .T. ) ;
#1754 =( GEOMETRIC_REPRESENTATION_CONTEXT ( 3 ) GLOBAL_UNCERTAINTY_ASSIGNED_CONTEXT ( ( #1447 ) ) GLOBAL_UNIT_ASSIGNED_CONTEXT ( ( #2588, #1392, #2132 ) ) REPRESENTATION_CONTEXT ( 'NONE', 'WORKASPACE' ) );
#1755 = ORIENTED_EDGE ( 'NONE', *, *, #657, .T. ) ;
#1756 = VERTEX_POINT ( 'NONE', #2638 ) ;
#1757 = ADVANCED_FACE ( 'NONE', ( #2503 ), #960, .F. ) ;
#1758 = FACE_OUTER_BOUND ( 'NONE', #1816, .T. ) ;
#1759 = DIRECTION ( 'NONE',  ( 1.000000000000000000, 0.000000000000000000, -0.000000000000000000 ) ) ;
#1760 = DIRECTION ( 'NONE',  ( -1.000000000000000000, 0.000000000000000000, -0.000000000000000000 ) ) ;
#1761 = FACE_OUTER_BOUND ( 'NONE', #352, .T. ) ;
#1762 = FACE_OUTER_BOUND ( 'NONE', #2830, .T. ) ;
#1763 = ORIENTED_EDGE ( 'NONE', *, *, #2556, .T. ) ;
#1764 = VECTOR ( 'NONE', #167, 1000.000000000000000 ) ;
#1765 = CIRCLE ( 'NONE', #2845, 1.425000000000000044 ) ;
#1766 = DIRECTION ( 'NONE',  ( 1.000000000000000000, 2.312964634635742957E-16, 0.000000000000000000 ) ) ;
#1767 = FILL_AREA_STYLE_COLOUR ( '', #901 ) ;
#1768 = DIRECTION ( 'NONE',  ( -1.000000000000000000, 0.000000000000000000, 0.000000000000000000 ) ) ;
#1769 = CARTESIAN_POINT ( 'NONE',  ( -37.00000000000000000, -5.785761963836251101E-15, 2.500000000000001332 ) ) ;
#1770 = ORIENTED_EDGE ( 'NONE', *, *, #2879, .T. ) ;
#1771 = ORIENTED_EDGE ( 'NONE', *, *, #220, .T. ) ;
#1772 = EDGE_CURVE ( 'NONE', #1108, #1178, #261, .T. ) ;
#1773 = DIRECTION ( 'NONE',  ( 1.000000000000000000, 0.000000000000000000, 0.000000000000000000 ) ) ;
#1774 = CARTESIAN_POINT ( 'NONE',  ( 37.66466167501431528, -1.348281052163420091, 16.39851580165996836 ) ) ;
#1775 = CARTESIAN_POINT ( 'NONE',  ( -37.00000000000000000, -9.935696797193021379E-15, 7.500000000000000000 ) ) ;
#1776 = ADVANCED_FACE ( 'NONE', ( #494, #1723 ), #1486, .F. ) ;
#1777 = CARTESIAN_POINT ( 'NONE',  ( 35.50000000000000711, 1.492884656567496302E-14, 20.99999999999999645 ) ) ;
#1778 = DIRECTION ( 'NONE',  ( 0.000000000000000000, -1.000000000000000000, 0.000000000000000000 ) ) ;
#1779 = VERTEX_POINT ( 'NONE', #736 ) ;
#1780 = AXIS2_PLACEMENT_3D ( 'NONE', #2535, #2039, #1612 ) ;
#1781 = CARTESIAN_POINT ( 'NONE',  ( 38.34772064623945909, 0.6658172387807621551, 16.47579882838004650 ) ) ;
#1782 = CARTESIAN_POINT ( 'NONE',  ( 155.0000000000000284, -6.928842772166554697E-15, 7.500000000000000000 ) ) ;
#1783 = DIRECTION ( 'NONE',  ( 1.000000000000000000, 2.312964634635742957E-16, 0.000000000000000000 ) ) ;
#1784 = AXIS2_PLACEMENT_3D ( 'NONE', #1714, #1741, #434 ) ;
#1785 = ORIENTED_EDGE ( 'NONE', *, *, #2945, .T. ) ;
#1786 = CARTESIAN_POINT ( 'NONE',  ( 0.000000000000000000, 0.000000000000000000, 1.499999999999999556 ) ) ;
#1787 = CARTESIAN_POINT ( 'NONE',  ( 35.50000000000000000, 1.243235838461289750E-14, 16.49999999999999289 ) ) ;
#1788 = DIRECTION ( 'NONE',  ( 0.000000000000000000, 0.000000000000000000, -1.000000000000000000 ) ) ;
#1789 = VERTEX_POINT ( 'NONE', #279 ) ;
#1790 = SHAPE_REPRESENTATION ( 'Graduated Stationary Sleeve Barrel', ( #2878 ), #603 ) ;
#1791 = DIRECTION ( 'NONE',  ( -0.000000000000000000, 0.5000000000000000000, 0.8660254037844385966 ) ) ;
#1792 = AXIS2_PLACEMENT_3D ( 'NONE', #1, #1511, #1560 ) ;
#1793 = EDGE_CURVE ( 'NONE', #1489, #2004, #1007, .T. ) ;
#1794 = DIRECTION ( 'NONE',  ( 1.000000000000000000, 0.000000000000000000, 0.000000000000000000 ) ) ;
#1795 = EDGE_LOOP ( 'NONE', ( #2032, #1358, #1497, #1411, #2892 ) ) ;
#1796 = VECTOR ( 'NONE', #1348, 1000.000000000000000 ) ;
#1797 = EDGE_CURVE ( 'NONE', #745, #2348, #155, .T. ) ;
#1798 = CARTESIAN_POINT ( 'NONE',  ( 35.65194399346782461, 0.6651260505907339304, 16.47584948644689007 ) ) ;
#1799 = CARTESIAN_POINT ( 'NONE',  ( 47.00000000000000000, 1.133017633246824530E-14, 7.500000000000000000 ) ) ;
#1800 = CARTESIAN_POINT ( 'NONE',  ( 180.0000000000000284, -6.928842772166554697E-15, 7.500000000000000000 ) ) ;
#1801 = VECTOR ( 'NONE', #2333, 1000.000000000000114 ) ;
#1802 = DIRECTION ( 'NONE',  ( 0.000000000000000000, 0.000000000000000000, -1.000000000000000000 ) ) ;
#1803 = VERTEX_POINT ( 'NONE', #528 ) ;
#1804 = FACE_OUTER_BOUND ( 'NONE', #1711, .T. ) ;
#1805 = DIRECTION ( 'NONE',  ( 0.000000000000000000, 0.000000000000000000, 1.000000000000000000 ) ) ;
#1806 = DIRECTION ( 'NONE',  ( 0.000000000000000000, 1.000000000000000000, 0.000000000000000000 ) ) ;
#1807 = ORIENTED_EDGE ( 'NONE', *, *, #1721, .F. ) ;
#1808 = CARTESIAN_POINT ( 'NONE',  ( 140.0000000000000000, -6.928842772166554697E-15, 20.50000000000000000 ) ) ;
#1809 = PRODUCT_DEFINITION_CONTEXT ( 'detailed design', #243, 'design' ) ;
#1810 = CARTESIAN_POINT ( 'NONE',  ( 140.0000000000000000, -5.336801933274995404E-15, -5.500000000000001776 ) ) ;
#1811 = ORIENTED_EDGE ( 'NONE', *, *, #2070, .T. ) ;
#1812 = EDGE_CURVE ( 'NONE', #2847, #2624, #2495, .T. ) ;
#1813 = LINE ( 'NONE', #2766, #2565 ) ;
#1814 = VECTOR ( 'NONE', #1923, 1000.000000000000000 ) ;
#1815 = SURFACE_STYLE_FILL_AREA ( #783 ) ;
#1816 = EDGE_LOOP ( 'NONE', ( #3075, #432 ) ) ;
#1817 = CARTESIAN_POINT ( 'NONE',  ( 36.07902659818449109, -1.200345445641969988, 16.42070378373878725 ) ) ;
#1818 = DIRECTION ( 'NONE',  ( -1.000000000000000000, 0.000000000000000000, -0.000000000000000000 ) ) ;
#1819 = EDGE_LOOP ( 'NONE', ( #451, #2655 ) ) ;
#1820 = CARTESIAN_POINT ( 'NONE',  ( 1.269999999999999796, 0.000000000000000000, 0.000000000000000000 ) ) ;
#1821 = EDGE_CURVE ( 'NONE', #576, #974, #1405, .T. ) ;
#1822 = DIRECTION ( 'NONE',  ( 0.000000000000000000, -1.224646799147353207E-16, 1.000000000000000000 ) ) ;
#1823 = VERTEX_POINT ( 'NONE', #1450 ) ;
#1824 = CARTESIAN_POINT ( 'NONE',  ( 35.69898883018239388, 0.7529305858385579864, 16.46882038169668050 ) ) ;
#1825 = AXIS2_PLACEMENT_3D ( 'NONE', #2933, #2996, #3194 ) ;
#1826 = ADVANCED_FACE ( 'NONE', ( #2240 ), #1224, .F. ) ;
#1827 = CARTESIAN_POINT ( 'NONE',  ( 155.0000000000000284, -6.928842772166554697E-15, 7.500000000000000000 ) ) ;
#1828 = MECHANICAL_DESIGN_GEOMETRIC_PRESENTATION_REPRESENTATION (  '', ( #1410 ), #801 ) ;
#1829 = VERTEX_POINT ( 'NONE', #1769 ) ;
#1830 = DIRECTION ( 'NONE',  ( -1.000000000000000000, -2.312964634635742957E-16, 0.000000000000000000 ) ) ;
#1831 = FACE_OUTER_BOUND ( 'NONE', #1749, .T. ) ;
#1832 = EDGE_LOOP ( 'NONE', ( #1145, #399, #2048, #117, #316 ) ) ;
#1833 = DIRECTION ( 'NONE',  ( 0.000000000000000000, 0.000000000000000000, 1.000000000000000000 ) ) ;
#1834 = DIRECTION ( 'NONE',  ( -0.000000000000000000, -0.000000000000000000, 1.000000000000000000 ) ) ;
#1835 = EDGE_LOOP ( 'NONE', ( #2410, #2151, #1307, #3160 ) ) ;
#1836 = LINE ( 'NONE', #2100, #58 ) ;
#1837 = DIRECTION ( 'NONE',  ( 1.000000000000000000, 0.000000000000000000, 0.000000000000000000 ) ) ;
#1838 = AXIS2_PLACEMENT_3D ( 'NONE', #256, #2515, #3043 ) ;
#1839 = CIRCLE ( 'NONE', #172, 8.999999999999994671 ) ;
#1840 = AXIS2_PLACEMENT_3D ( 'NONE', #331, #1783, #1518 ) ;
#1841 = PLANE ( 'NONE',  #3081 ) ;
#1842 = ORIENTED_EDGE ( 'NONE', *, *, #147, .T. ) ;
#1843 = CIRCLE ( 'NONE', #121, 14.00000000000000000 ) ;
#1844 = AXIS2_PLACEMENT_3D ( 'NONE', #2486, #1298, #3049 ) ;
#1845 = ADVANCED_FACE ( 'NONE', ( #2254 ), #9, .F. ) ;
#1846 = DIRECTION ( 'NONE',  ( 1.000000000000000000, -0.000000000000000000, -0.000000000000000000 ) ) ;
#1847 = CARTESIAN_POINT ( 'NONE',  ( 38.30993956269965395, -0.7564481093111403709, 16.46997477067511539 ) ) ;
#1848 = B_SPLINE_CURVE_WITH_KNOTS ( 'NONE', 3,
 ( #689, #196, #1416, #676, #1179, #1942, #2920, #1399, #2365, #1193, #2652, #429, #2865, #625, #1690, #1930, #2125, #1620, #2190, #448, #3175, #942, #143, #876 ),
 .UNSPECIFIED., .F., .F.,
 ( 4, 2, 2, 2, 2, 2, 2, 2, 2, 2, 2, 4 ),
 ( 0.004697885398315436792, 0.005284974574641427766, 0.005872063750967418741, 0.006165608339130407289, 0.006459152927293394103, 0.007046242103619369465, 0.007339786691782357146, 0.007633331279945343960, 0.007926875868108331641, 0.008220420456271318455, 0.008807509632597295551, 0.009394598808923269179 ),
 .UNSPECIFIED. ) ;
#1849 = VERTEX_POINT ( 'NONE', #724 ) ;
#1850 = APPLICATION_CONTEXT ( 'automotive_design' ) ;
#1851 = FACE_OUTER_BOUND ( 'NONE', #2388, .T. ) ;
#1852 = CARTESIAN_POINT ( 'NONE',  ( 60.00000000000000000, -6.928842772166554697E-15, 7.500000000000000000 ) ) ;
#1853 = LINE ( 'NONE', #2629, #1132 ) ;
#1854 =( LENGTH_UNIT ( ) NAMED_UNIT ( * ) SI_UNIT ( .MILLI., .METRE. ) );
#1855 = EDGE_LOOP ( 'NONE', ( #2272, #1610 ) ) ;
#1856 = ORIENTED_EDGE ( 'NONE', *, *, #947, .T. ) ;
#1857 = LINE ( 'NONE', #2356, #2296 ) ;
#1858 = CARTESIAN_POINT ( 'NONE',  ( -5.000000000000000000, -6.928842772166554697E-15, 7.500000000000000000 ) ) ;
#1859 = CYLINDRICAL_SURFACE ( 'NONE', #900, 41.99999999999999289 ) ;
#1860 = VERTEX_POINT ( 'NONE', #2009 ) ;
#1861 = AXIS2_PLACEMENT_3D ( 'NONE', #1887, #1573, #1625 ) ;
#1862 = ORIENTED_EDGE ( 'NONE', *, *, #2720, .T. ) ;
#1863 = AXIS2_PLACEMENT_3D ( 'NONE', #1384, #1674, #3108 ) ;
#1864 = CARTESIAN_POINT ( 'NONE',  ( 37.41786025882474576, -7.616137346557303354E-15, 12.50000000000000000 ) ) ;
#1865 = EDGE_CURVE ( 'NONE', #516, #548, #578, .T. ) ;
#1866 = VERTEX_POINT ( 'NONE', #2978 ) ;
#1867 = PLANE ( 'NONE',  #1950 ) ;
#1868 = DIRECTION ( 'NONE',  ( 0.000000000000000000, 0.000000000000000000, 1.000000000000000000 ) ) ;
#1869 = EDGE_CURVE ( 'NONE', #91, #2427, #1878, .T. ) ;
#1870 = DIRECTION ( 'NONE',  ( 0.000000000000000000, 0.000000000000000000, 1.000000000000000000 ) ) ;
#1871 = EDGE_LOOP ( 'NONE', ( #2504, #602, #513, #2804 ) ) ;
#1872 = ORIENTED_EDGE ( 'NONE', *, *, #1104, .T. ) ;
#1873 = CYLINDRICAL_SURFACE ( 'NONE', #2446, 1.499999999999994449 ) ;
#1874 = PRODUCT_DEFINITION_SHAPE ( 'NONE', 'NONE',  #3228 ) ;
#1875 = CARTESIAN_POINT ( 'NONE',  ( 3.469446951953614189E-15, -15.00000000000000355, 15.00000000000000000 ) ) ;
#1876 = DIRECTION ( 'NONE',  ( -0.000000000000000000, -0.000000000000000000, -1.000000000000000000 ) ) ;
#1877 = VERTEX_POINT ( 'NONE', #973 ) ;
#1878 = CIRCLE ( 'NONE', #473, 10.00000000000000178 ) ;
#1879 = UNCERTAINTY_MEASURE_WITH_UNIT (LENGTH_MEASURE( 1.000000000000000082E-05 ), #776, 'distance_accuracy_value', 'NONE');
#1880 = CARTESIAN_POINT ( 'NONE',  ( 41.99999999999999289, -13.99999999999999112, 7.500000000000001776 ) ) ;
#1881 = MECHANICAL_DESIGN_GEOMETRIC_PRESENTATION_REPRESENTATION (  '', ( #881 ), #1566 ) ;
#1882 = VERTEX_POINT ( 'NONE', #1708 ) ;
#1883 = CARTESIAN_POINT ( 'NONE',  ( 37.21226234515645359, 0.3528290111407958451, 12.48804596179740756 ) ) ;
#1884 = ORIENTED_EDGE ( 'NONE', *, *, #3136, .T. ) ;
#1885 = CARTESIAN_POINT ( 'NONE',  ( 0.000000000000000000, 0.5773502691896263972, 1.000000000000000000 ) ) ;
#1886 = EDGE_CURVE ( 'NONE', #1604, #2350, #1618, .T. ) ;
#1887 = CARTESIAN_POINT ( 'NONE',  ( 37.00000000000000000, 1.474514954580286030E-14, 20.99999999999999645 ) ) ;
#1888 = VECTOR ( 'NONE', #2166, 1000.000000000000000 ) ;
#1889 = ORIENTED_EDGE ( 'NONE', *, *, #2322, .T. ) ;
#1890 = VERTEX_POINT ( 'NONE', #1205 ) ;
#1891 = DIRECTION ( 'NONE',  ( 0.000000000000000000, 0.000000000000000000, 1.000000000000000000 ) ) ;
#1892 = EDGE_CURVE ( 'NONE', #861, #403, #2205, .T. ) ;
#1893 = CYLINDRICAL_SURFACE ( 'NONE', #2979, 5.000000000000000000 ) ;
#1894 = UNCERTAINTY_MEASURE_WITH_UNIT (LENGTH_MEASURE( 1.000000000000000082E-05 ), #557, 'distance_accuracy_value', 'NONE');
#1895 = CIRCLE ( 'NONE', #2357, 1.000000000000000000 ) ;
#1896 = CARTESIAN_POINT ( 'NONE',  ( -41.99999999999999289, -15.00000000000000711, 15.00000000000000000 ) ) ;
#1897 = ORIENTED_EDGE ( 'NONE', *, *, #540, .F. ) ;
#1898 = PLANE ( 'NONE',  #2748 ) ;
#1899 = STYLED_ITEM ( 'NONE', ( #1036 ), #1050 ) ;
#1900 = CIRCLE ( 'NONE', #390, 4.999999999999999112 ) ;
#1901 = ORIENTED_EDGE ( 'NONE', *, *, #2191, .F. ) ;
#1902 = CARTESIAN_POINT ( 'NONE',  ( 140.0000000000000000, -6.928842772166554697E-15, 7.500000000000000000 ) ) ;
#1903 = AXIS2_PLACEMENT_3D ( 'NONE', #1210, #1505, #2449 ) ;
#1904 = VERTEX_POINT ( 'NONE', #2458 ) ;
#1905 = DIRECTION ( 'NONE',  ( -0.000000000000000000, -1.000000000000000000, -0.000000000000000000 ) ) ;
#1906 = CARTESIAN_POINT ( 'NONE',  ( 41.99999999999999289, 6.449497959004948951E-15, 0.000000000000000000 ) ) ;
#1907 = AXIS2_PLACEMENT_3D ( 'NONE', #2630, #2372, #356 ) ;
#1908 = ORIENTED_EDGE ( 'NONE', *, *, #2164, .T. ) ;
#1909 = CARTESIAN_POINT ( 'NONE',  ( 27.00000000000000000, 1.133017633246824530E-14, 7.500000000000000000 ) ) ;
#1910 = PRODUCT_DEFINITION_FORMATION_WITH_SPECIFIED_SOURCE ( 'ANY', '', #2771, .NOT_KNOWN. ) ;
#1911 = FACE_OUTER_BOUND ( 'NONE', #1565, .T. ) ;
#1912 = EDGE_CURVE ( 'NONE', #2818, #79, #477, .T. ) ;
#1913 = DIRECTION ( 'NONE',  ( 2.312964634635742957E-16, -1.000000000000000000, 0.000000000000000000 ) ) ;
#1914 = ORIENTED_EDGE ( 'NONE', *, *, #718, .F. ) ;
#1915 = DIRECTION ( 'NONE',  ( -1.000000000000000000, -0.000000000000000000, -0.000000000000000000 ) ) ;
#1916 = VERTEX_POINT ( 'NONE', #2962 ) ;
#1917 = PRESENTATION_STYLE_ASSIGNMENT (( #527 ) ) ;
#1918 = ORIENTED_EDGE ( 'NONE', *, *, #1821, .T. ) ;
#1919 = DIRECTION ( 'NONE',  ( 0.000000000000000000, 0.000000000000000000, -1.000000000000000000 ) ) ;
#1920 = UNCERTAINTY_MEASURE_WITH_UNIT (LENGTH_MEASURE( 1.000000000000000082E-05 ), #1479, 'distance_accuracy_value', 'NONE');
#1921 = VECTOR ( 'NONE', #2306, 1000.000000000000000 ) ;
#1922 = CARTESIAN_POINT ( 'NONE',  ( 27.00000000000000000, -3.708099243547831048, 20.99999999999999645 ) ) ;
#1923 = DIRECTION ( 'NONE',  ( 1.000000000000000000, -0.000000000000000000, -0.000000000000000000 ) ) ;
#1924 = DIRECTION ( 'NONE',  ( 0.000000000000000000, 0.000000000000000000, -1.000000000000000000 ) ) ;
#1925 = ORIENTED_EDGE ( 'NONE', *, *, #298, .T. ) ;
#1926 = FILL_AREA_STYLE ('',( #455 ) ) ;
#1927 = DIRECTION ( 'NONE',  ( -0.5000000000000042188, 0.000000000000000000, 0.8660254037844361541 ) ) ;
#1928 = DIRECTION ( 'NONE',  ( -1.000000000000000000, -2.312964634635743450E-16, -0.000000000000000000 ) ) ;
#1929 = ORIENTED_EDGE ( 'NONE', *, *, #2879, .F. ) ;
#1930 = CARTESIAN_POINT ( 'NONE',  ( 37.66466167501430107, 1.348281052163445404, 16.39851580165995415 ) ) ;
#1931 = EDGE_CURVE ( 'NONE', #2350, #1604, #1300, .T. ) ;
#1932 = EDGE_LOOP ( 'NONE', ( #2500, #2163, #262, #1897 ) ) ;
#1933 = DIRECTION ( 'NONE',  ( -0.000000000000000000, 0.000000000000000000, 1.000000000000000000 ) ) ;
#1934 = ORIENTED_EDGE ( 'NONE', *, *, #2782, .F. ) ;
#1935 = DIRECTION ( 'NONE',  ( 0.000000000000000000, 0.000000000000000000, -1.000000000000000000 ) ) ;
#1936 = DIRECTION ( 'NONE',  ( 0.000000000000000000, 0.000000000000000000, 1.000000000000000000 ) ) ;
#1937 = LINE ( 'NONE', #696, #2579 ) ;
#1938 = PRODUCT_CONTEXT ( 'NONE', #1577, 'mechanical' ) ;
#1939 = LINE ( 'NONE', #472, #1943 ) ;
#1940 = VECTOR ( 'NONE', #3203, 1000.000000000000000 ) ;
#1941 = LINE ( 'NONE', #958, #1951 ) ;
#1942 = CARTESIAN_POINT ( 'NONE',  ( 36.00776062886353657, 1.129166992945610737, 16.42915638304272008 ) ) ;
#1943 = VECTOR ( 'NONE', #700, 1000.000000000000000 ) ;
#1944 = VERTEX_POINT ( 'NONE', #887 ) ;
#1945 = DIRECTION ( 'NONE',  ( 0.000000000000000000, 0.000000000000000000, -1.000000000000000000 ) ) ;
#1946 = ORIENTED_EDGE ( 'NONE', *, *, #1227, .T. ) ;
#1947 = CIRCLE ( 'NONE', #2102, 7.500000000000000000 ) ;
#1948 = ADVANCED_FACE ( 'NONE', ( #313 ), #297, .T. ) ;
#1949 = LINE ( 'NONE', #404, #1465 ) ;
#1950 = AXIS2_PLACEMENT_3D ( 'NONE', #2066, #2851, #629 ) ;
#1951 = VECTOR ( 'NONE', #2702, 1000.000000000000000 ) ;
#1952 = PLANE ( 'NONE',  #551 ) ;
#1953 = DIRECTION ( 'NONE',  ( 0.000000000000000000, 0.000000000000000000, 1.000000000000000000 ) ) ;
#1954 = CARTESIAN_POINT ( 'NONE',  ( 1.649999999999999911, 0.000000000000000000, 0.000000000000000000 ) ) ;
#1955 = CIRCLE ( 'NONE', #445, 1.499999999999999778 ) ;
#1956 = CIRCLE ( 'NONE', #1373, 1.599999999999999645 ) ;
#1957 =( GEOMETRIC_REPRESENTATION_CONTEXT ( 3 ) GLOBAL_UNCERTAINTY_ASSIGNED_CONTEXT ( ( #873 ) ) GLOBAL_UNIT_ASSIGNED_CONTEXT ( ( #3007, #3022, #309 ) ) REPRESENTATION_CONTEXT ( 'NONE', 'WORKASPACE' ) );
#1958 = DIRECTION ( 'NONE',  ( 0.000000000000000000, 0.000000000000000000, -1.000000000000000000 ) ) ;
#1959 =( LENGTH_UNIT ( ) NAMED_UNIT ( * ) SI_UNIT ( .MILLI., .METRE. ) );
#1960 = ADVANCED_FACE ( 'NONE', ( #2632 ), #2841, .T. ) ;
#1961 = DIRECTION ( 'NONE',  ( -1.000000000000000000, 0.000000000000000000, 0.000000000000000000 ) ) ;
#1962 = CARTESIAN_POINT ( 'NONE',  ( 140.0000000000000000, -6.928842772166554697E-15, 7.500000000000000000 ) ) ;
#1963 = ORIENTED_EDGE ( 'NONE', *, *, #1243, .T. ) ;
#1964 = VERTEX_POINT ( 'NONE', #1379 ) ;
#1965 = DIRECTION ( 'NONE',  ( 1.000000000000000000, 0.000000000000000000, 0.000000000000000000 ) ) ;
#1966 = CARTESIAN_POINT ( 'NONE',  ( -5.000000000000000000, -6.928842772166554697E-15, 7.500000000000000000 ) ) ;
#1967 = FACE_OUTER_BOUND ( 'NONE', #232, .T. ) ;
#1968 = DIRECTION ( 'NONE',  ( 0.000000000000000000, 0.000000000000000000, 1.000000000000000000 ) ) ;
#1969 = APPLICATION_PROTOCOL_DEFINITION ( 'draft international standard', 'automotive_design', 1998, #2078 ) ;
#1970 = AXIS2_PLACEMENT_3D ( 'NONE', #93, #342, #821 ) ;
#1971 = ADVANCED_FACE ( 'NONE', ( #653, #2135 ), #3028, .F. ) ;
#1972 = CARTESIAN_POINT ( 'NONE',  ( 27.00000000000000000, -7.622732162557277534E-15, 7.500000000000000000 ) ) ;
#1973 = PRODUCT_DEFINITION_SHAPE ( 'NONE', 'NONE',  #3227 ) ;
#1974 = SURFACE_SIDE_STYLE ('',( #3190 ) ) ;
#1975 = CARTESIAN_POINT ( 'NONE',  ( -23.99999999999999645, -6.928842772166554697E-15, 7.500000000000000000 ) ) ;
#1976 = CARTESIAN_POINT ( 'NONE',  ( 155.0000000000000284, -6.928842772166554697E-15, 7.500000000000000000 ) ) ;
#1977 = ORIENTED_EDGE ( 'NONE', *, *, #893, .F. ) ;
#1978 = ORIENTED_EDGE ( 'NONE', *, *, #943, .T. ) ;
#1979 = CARTESIAN_POINT ( 'NONE',  ( 27.00000000000000000, -7.622732162557277534E-15, 12.50000000000000000 ) ) ;
#1980 = DIRECTION ( 'NONE',  ( -0.000000000000000000, -0.000000000000000000, 1.000000000000000000 ) ) ;
#1981 = CARTESIAN_POINT ( 'NONE',  ( 36.89323119352727787, -0.3922100905875090526, 12.48459338812192776 ) ) ;
#1982 = CONTEXT_DEPENDENT_SHAPE_REPRESENTATION ( #109, #1739 ) ;
#1983 = AXIS2_PLACEMENT_3D ( 'NONE', #1502, #988, #2717 ) ;
#1984 = DIRECTION ( 'NONE',  ( -0.000000000000000000, -0.000000000000000000, 1.000000000000000000 ) ) ;
#1985 = AXIS2_PLACEMENT_3D ( 'NONE', #1153, #1186, #1460 ) ;
#1986 = EDGE_LOOP ( 'NONE', ( #2461, #961, #1732, #999 ) ) ;
#1987 = ADVANCED_FACE ( 'NONE', ( #620 ), #2141, .T. ) ;
#1988 = PRODUCT_RELATED_PRODUCT_CATEGORY ( 'part', '', ( #2954 ) ) ;
#1989 = DIRECTION ( 'NONE',  ( -1.000000000000000000, -0.000000000000000000, -0.000000000000000000 ) ) ;
#1990 = CIRCLE ( 'NONE', #268, 8.999999999999992895 ) ;
#1991 = ADVANCED_FACE ( 'NONE', ( #2592 ), #2120, .T. ) ;
#1992 = DIRECTION ( 'NONE',  ( 0.000000000000000000, 1.000000000000000000, 0.000000000000000000 ) ) ;
#1993 = ORIENTED_EDGE ( 'NONE', *, *, #192, .T. ) ;
#1994 = EDGE_LOOP ( 'NONE', ( #2692, #2519 ) ) ;
#1995 = CARTESIAN_POINT ( 'NONE',  ( 47.00000000000000000, 1.133017633246824530E-14, 7.500000000000000000 ) ) ;
#1996 = CARTESIAN_POINT ( 'NONE',  ( 37.19571985532142833, -1.490394421081172371, 16.37575894629745932 ) ) ;
#1997 = CARTESIAN_POINT ( 'NONE',  ( 47.00000000000000000, 1.133017633246824530E-14, -1.499999999999989120 ) ) ;
#1998 = AXIS2_PLACEMENT_3D ( 'NONE', #239, #486, #2471 ) ;
#1999 = ITEM_DEFINED_TRANSFORMATION ( 'NONE', 'NONE', #3145,  #2878 ) ;
#2000 = CARTESIAN_POINT ( 'NONE',  ( 140.0000000000000000, -6.928842772166554697E-15, 12.50000000000000000 ) ) ;
#2001 =( NAMED_UNIT ( * ) SI_UNIT ( $, .STERADIAN. ) SOLID_ANGLE_UNIT ( ) );
#2002 = VECTOR ( 'NONE', #1195, 1000.000000000000000 ) ;
#2003 = AXIS2_PLACEMENT_3D ( 'NONE', #89, #2075, #300 ) ;
#2004 = VERTEX_POINT ( 'NONE', #2767 ) ;
#2005 = CARTESIAN_POINT ( 'NONE',  ( 1.040000000000000036, -0.8660254037844382635, 0.5000000000000002220 ) ) ;
#2006 = EDGE_CURVE ( 'NONE', #79, #391, #45, .T. ) ;
#2007 = CARTESIAN_POINT ( 'NONE',  ( 1.649999999999999911, 1.499999999999999112, 0.000000000000000000 ) ) ;
#2008 = DIRECTION ( 'NONE',  ( 1.000000000000000000, 0.000000000000000000, 0.000000000000000000 ) ) ;
#2009 = CARTESIAN_POINT ( 'NONE',  ( 1.040000000000000036, -0.5773502691896253980, 1.000000000000000000 ) ) ;
#2010 = ADVANCED_FACE ( 'NONE', ( #1394 ), #544, .T. ) ;
#2011 = ORIENTED_EDGE ( 'NONE', *, *, #2422, .F. ) ;
#2012 = ORIENTED_EDGE ( 'NONE', *, *, #3136, .F. ) ;
#2013 = DIRECTION ( 'NONE',  ( 0.000000000000000000, 0.000000000000000000, 1.000000000000000000 ) ) ;
#2014 = CARTESIAN_POINT ( 'NONE',  ( 30.00000000000000000, 7.398136453587482028E-15, 7.500000000000000000 ) ) ;
#2015 = DIRECTION ( 'NONE',  ( 0.000000000000000000, 0.000000000000000000, 1.000000000000000000 ) ) ;
#2016 = DIRECTION ( 'NONE',  ( 1.000000000000000000, 2.312964634635742957E-16, 0.000000000000000000 ) ) ;
#2017 = UNCERTAINTY_MEASURE_WITH_UNIT (LENGTH_MEASURE( 1.000000000000000082E-05 ), #605, 'distance_accuracy_value', 'NONE');
#2018 = DIRECTION ( 'NONE',  ( 1.000000000000000000, -0.000000000000000000, -0.000000000000000000 ) ) ;
#2019 = ORIENTED_EDGE ( 'NONE', *, *, #2921, .F. ) ;
#2020 = AXIS2_PLACEMENT_3D ( 'NONE', #3186, #203, #716 ) ;
#2021 = AXIS2_PLACEMENT_3D ( 'NONE', #1029, #806, #251 ) ;
#2022 = CARTESIAN_POINT ( 'NONE',  ( 38.49023808469348751, 0.1968962347057520990, 16.49835841594091335 ) ) ;
#2023 = FILL_AREA_STYLE ('',( #826 ) ) ;
#2024 = DIRECTION ( 'NONE',  ( 2.312964634635742957E-16, -1.000000000000000000, 0.000000000000000000 ) ) ;
#2025 = LINE ( 'NONE', #800, #1003 ) ;
#2026 = AXIS2_PLACEMENT_3D ( 'NONE', #1391, #1327, #1868 ) ;
#2027 = ORIENTED_EDGE ( 'NONE', *, *, #2298, .F. ) ;
#2028 = ADVANCED_FACE ( 'NONE', ( #871 ), #2375, .F. ) ;
#2029 = LINE ( 'NONE', #334, #803 ) ;
#2030 = CARTESIAN_POINT ( 'NONE',  ( 1.040000000000000036, 0.5773502691896263972, -1.000000000000000000 ) ) ;
#2031 = LINE ( 'NONE', #2480, #1337 ) ;
#2032 = ORIENTED_EDGE ( 'NONE', *, *, #525, .T. ) ;
#2033 = EDGE_CURVE ( 'NONE', #1503, #1789, #2524, .T. ) ;
#2034 = DIRECTION ( 'NONE',  ( 0.000000000000000000, 1.000000000000000000, 0.000000000000000000 ) ) ;
#2035 = CARTESIAN_POINT ( 'NONE',  ( 27.00000000000000000, -6.520550043324659623E-15, -1.499999999999992673 ) ) ;
#2036 = ORIENTED_EDGE ( 'NONE', *, *, #2701, .T. ) ;
#2037 = VERTEX_POINT ( 'NONE', #41 ) ;
#2038 = CARTESIAN_POINT ( 'NONE',  ( 37.75516277711826518, 1.310683246666518365, 16.40437238582925872 ) ) ;
#2039 = DIRECTION ( 'NONE',  ( -1.000000000000000000, -0.000000000000000000, -0.000000000000000000 ) ) ;
#2040 = ADVANCED_FACE ( 'NONE', ( #1037 ), #1873, .F. ) ;
#2041 =( NAMED_UNIT ( * ) SI_UNIT ( $, .STERADIAN. ) SOLID_ANGLE_UNIT ( ) );
#2042 = AXIS2_PLACEMENT_3D ( 'NONE', #166, #2182, #2956 ) ;
#2043 = ORIENTED_EDGE ( 'NONE', *, *, #2828, .T. ) ;
#2044 = CARTESIAN_POINT ( 'NONE',  ( 155.0000000000000284, -6.928842772166554697E-15, 7.500000000000000000 ) ) ;
#2045 = CARTESIAN_POINT ( 'NONE',  ( 37.75078578997759848, -1.302282315510294941, 16.40545230064624249 ) ) ;
#2046 = FACE_OUTER_BOUND ( 'NONE', #1819, .T. ) ;
#2047 = EDGE_CURVE ( 'NONE', #1849, #169, #3120, .T. ) ;
#2048 = ORIENTED_EDGE ( 'NONE', *, *, #2489, .T. ) ;
#2049 = PRODUCT_RELATED_PRODUCT_CATEGORY ( 'part', '', ( #2285 ) ) ;
#2050 = CARTESIAN_POINT ( 'NONE',  ( 27.00000000000000355, -13.99999999999999289, 7.500000000000001776 ) ) ;
#2051 = AXIS2_PLACEMENT_3D ( 'NONE', #2685, #1731, #2647 ) ;
#2052 = SURFACE_SIDE_STYLE ('',( #2278 ) ) ;
#2053 = ORIENTED_EDGE ( 'NONE', *, *, #2322, .F. ) ;
#2054 = COLOUR_RGB ( '',1.000000000000000000, 0.9490196078431372140, 0.9098039215686274384 ) ;
#2055 = CARTESIAN_POINT ( 'NONE',  ( 36.61043004145793134, 1.451850406891378675, 16.38214551140935882 ) ) ;
#2056 = AXIS2_PLACEMENT_3D ( 'NONE', #1603, #2368, #1089 ) ;
#2057 = CARTESIAN_POINT ( 'NONE',  ( 1.040000000000000036, 1.154700538379252350, -1.084202172485497162E-16 ) ) ;
#2058 = DIRECTION ( 'NONE',  ( 1.000000000000000000, 0.000000000000000000, 0.000000000000000000 ) ) ;
#2059 = MECHANICAL_DESIGN_GEOMETRIC_PRESENTATION_REPRESENTATION (  '', ( #2940 ), #3047 ) ;
#2060 = ORIENTED_EDGE ( 'NONE', *, *, #1080, .F. ) ;
#2061 = ORIENTED_EDGE ( 'NONE', *, *, #2639, .T. ) ;
#2062 = EDGE_CURVE ( 'NONE', #1393, #1599, #1857, .T. ) ;
#2063 = CARTESIAN_POINT ( 'NONE',  ( 35.86950496355627394, -0.9908260551213471379, 16.44556929574714133 ) ) ;
#2064 = FACE_OUTER_BOUND ( 'NONE', #569, .T. ) ;
#2065 = ORIENTED_EDGE ( 'NONE', *, *, #799, .F. ) ;
#2066 = CARTESIAN_POINT ( 'NONE',  ( 41.99999999999999289, 6.449497959004948951E-15, 15.00000000000000000 ) ) ;
#2067 = CARTESIAN_POINT ( 'NONE',  ( 27.00000000000000355, -11.82159041753688200, 0.000000000000000000 ) ) ;
#2068 = FILL_AREA_STYLE ('',( #292 ) ) ;
#2069 = EDGE_LOOP ( 'NONE', ( #2311, #2475, #2472, #199, #336 ) ) ;
#2070 = EDGE_CURVE ( 'NONE', #2689, #2974, #1730, .T. ) ;
#2071 = CARTESIAN_POINT ( 'NONE',  ( 35.50000000000000711, 1.492884656567496302E-14, 20.99999999999999645 ) ) ;
#2072 = AXIS2_PLACEMENT_3D ( 'NONE', #2758, #17, #775 ) ;
#2073 = DIRECTION ( 'NONE',  ( 0.000000000000000000, 1.000000000000000000, 0.000000000000000000 ) ) ;
#2074 = EDGE_LOOP ( 'NONE', ( #2, #1106, #2963, #1141 ) ) ;
#2075 = DIRECTION ( 'NONE',  ( 1.000000000000000000, -0.000000000000000000, -0.000000000000000000 ) ) ;
#2076 = DIRECTION ( 'NONE',  ( -1.000000000000000000, -0.000000000000000000, -0.000000000000000000 ) ) ;
#2077 = VERTEX_POINT ( 'NONE', #2609 ) ;
#2078 = APPLICATION_CONTEXT ( 'automotive_design' ) ;
#2079 = DIRECTION ( 'NONE',  ( 1.000000000000000000, 0.000000000000000000, 0.000000000000000000 ) ) ;
#2080 = SHAPE_REPRESENTATION ( 'Rotary Thimble Outer Sleeve', ( #2878 ), #2989 ) ;
#2081 = CARTESIAN_POINT ( 'NONE',  ( 41.99999999999999289, -15.00000000000000355, 15.00000000000000000 ) ) ;
#2082 = ORIENTED_EDGE ( 'NONE', *, *, #234, .T. ) ;
#2083 = DIRECTION ( 'NONE',  ( -0.000000000000000000, 0.5000000000000000000, 0.8660254037844385966 ) ) ;
#2084 = EDGE_CURVE ( 'NONE', #585, #1570, #530, .T. ) ;
#2085 = AXIS2_PLACEMENT_3D ( 'NONE', #1020, #1466, #1992 ) ;
#2086 = ADVANCED_FACE ( 'NONE', ( #698 ), #206, .F. ) ;
#2087 = ORIENTED_EDGE ( 'NONE', *, *, #101, .F. ) ;
#2088 = VERTEX_POINT ( 'NONE', #422 ) ;
#2089 = CIRCLE ( 'NONE', #2600, 14.00000000000000000 ) ;
#2090 = CARTESIAN_POINT ( 'NONE',  ( 37.19662223785018540, -1.499925442620293259, 16.37413227714581510 ) ) ;
#2091 = DIRECTION ( 'NONE',  ( 0.000000000000000000, 0.000000000000000000, -1.000000000000000000 ) ) ;
#2092 = VERTEX_POINT ( 'NONE', #2170 ) ;
#2093 = DIRECTION ( 'NONE',  ( 1.000000000000000000, 0.000000000000000000, 0.000000000000000000 ) ) ;
#2094 = DIRECTION ( 'NONE',  ( -1.000000000000000000, -0.000000000000000000, -0.000000000000000000 ) ) ;
#2095 = SHAPE_DEFINITION_REPRESENTATION ( #2977, #2080 ) ;
#2096 = EDGE_LOOP ( 'NONE', ( #1289, #1158, #3023, #2650, #1402 ) ) ;
#2097 = ORIENTED_EDGE ( 'NONE', *, *, #943, .F. ) ;
#2098 = CIRCLE ( 'NONE', #1161, 5.000000000000000000 ) ;
#2099 = MANIFOLD_SOLID_BREP ( 'Boss-Extrude1', #112 ) ;
#2100 = CARTESIAN_POINT ( 'NONE',  ( 155.0000000000000284, -5.949125332848671934E-15, -0.5000000000000004441 ) ) ;
#2101 = SURFACE_SIDE_STYLE ('',( #3156 ) ) ;
#2102 = AXIS2_PLACEMENT_3D ( 'NONE', #3030, #3051, #2549 ) ;
#2103 = CIRCLE ( 'NONE', #2514, 5.000000000000000000 ) ;
#2104 = ADVANCED_FACE ( 'NONE', ( #3154 ), #476, .F. ) ;
#2105 = MANIFOLD_SOLID_BREP ( 'Boss-Extrude1', #61 ) ;
#2106 = LINE ( 'NONE', #1896, #1639 ) ;
#2107 = ORIENTED_EDGE ( 'NONE', *, *, #2006, .F. ) ;
#2108=STYLED_ITEM('',(#3243),#3178);
#2109 = VECTOR ( 'NONE', #2083, 1000.000000000000227 ) ;
#2110 = EDGE_CURVE ( 'NONE', #1108, #1890, #157, .T. ) ;
#2111 = STYLED_ITEM ( 'NONE', ( #21 ), #1139 ) ;
#2112 = EDGE_LOOP ( 'NONE', ( #1737, #384, #1963, #2848 ) ) ;
#2113 = LINE ( 'NONE', #1370, #1008 ) ;
#2114 = ORIENTED_EDGE ( 'NONE', *, *, #207, .T. ) ;
#2115 = CARTESIAN_POINT ( 'NONE',  ( 100.0000000000000000, -6.928842772166554697E-15, 7.500000000000000000 ) ) ;
#2116 = FACE_OUTER_BOUND ( 'NONE', #1419, .T. ) ;
#2117 = APPLICATION_PROTOCOL_DEFINITION ( 'draft international standard', 'automotive_design', 1998, #808 ) ;
#2118 = VERTEX_POINT ( 'NONE', #1429 ) ;
#2119 = EDGE_LOOP ( 'NONE', ( #293, #1143 ) ) ;
#2120 = CYLINDRICAL_SURFACE ( 'NONE', #1459, 10.00000000000000178 ) ;
#2121 = CARTESIAN_POINT ( 'NONE',  ( 0.000000000000000000, 0.5773502691896263972, 1.000000000000000000 ) ) ;
#2122 = DIRECTION ( 'NONE',  ( 1.000000000000000000, 0.000000000000000000, 0.000000000000000000 ) ) ;
#2123 = ORIENTED_EDGE ( 'NONE', *, *, #3014, .T. ) ;
#2124 = AXIS2_PLACEMENT_3D ( 'NONE', #1260, #2018, #3006 ) ;
#2125 = CARTESIAN_POINT ( 'NONE',  ( 37.75078578997757717, 1.302282315510324029, 16.40545230064623183 ) ) ;
#2126 = ORIENTED_EDGE ( 'NONE', *, *, #559, .F. ) ;
#2127 = CYLINDRICAL_SURFACE ( 'NONE', #703, 13.00000000000000178 ) ;
#2128 = ORIENTED_EDGE ( 'NONE', *, *, #372, .T. ) ;
#2129 = EDGE_CURVE ( 'NONE', #401, #1849, #1151, .T. ) ;
#2130 = CARTESIAN_POINT ( 'NONE',  ( 155.0000000000000284, -6.928842772166554697E-15, 7.500000000000000000 ) ) ;
#2131 = DIRECTION ( 'NONE',  ( 1.000000000000000000, 2.312964634635742957E-16, 0.000000000000000000 ) ) ;
#2132 =( NAMED_UNIT ( * ) SI_UNIT ( $, .STERADIAN. ) SOLID_ANGLE_UNIT ( ) );
#2133 = EDGE_LOOP ( 'NONE', ( #1261, #892 ) ) ;
#2134 = ORIENTED_EDGE ( 'NONE', *, *, #2976, .F. ) ;
#2135 = FACE_BOUND ( 'NONE', #2178, .T. ) ;
#2136 = MANIFOLD_SOLID_BREP ( 'Cut-Extrude-Thin1', #443 ) ;
#2137 = DIRECTION ( 'NONE',  ( 1.000000000000000000, 0.000000000000000000, 0.000000000000000000 ) ) ;
#2138 =( NAMED_UNIT ( * ) PLANE_ANGLE_UNIT ( ) SI_UNIT ( $, .RADIAN. ) );
#2139 = CARTESIAN_POINT ( 'NONE',  ( 60.00000000000000000, -5.520498953147098126E-15, 18.50000000000000355 ) ) ;
#2140 = ORIENTED_EDGE ( 'NONE', *, *, #2308, .T. ) ;
#2141 = CONICAL_SURFACE ( 'NONE', #3068, 12.00000000000000000, 0.09966865249115851311 ) ;
#2142 = DIRECTION ( 'NONE',  ( 0.000000000000000000, 0.000000000000000000, 1.000000000000000000 ) ) ;
#2143 = ORIENTED_EDGE ( 'NONE', *, *, #1525, .F. ) ;
#2144 = DIRECTION ( 'NONE',  ( -1.000000000000000000, -0.000000000000000000, -0.000000000000000000 ) ) ;
#2145 = ORIENTED_EDGE ( 'NONE', *, *, #1931, .F. ) ;
#2146 = DIRECTION ( 'NONE',  ( -1.000000000000000000, -2.312964634635742957E-16, 0.000000000000000000 ) ) ;
#2147 = EDGE_CURVE ( 'NONE', #1134, #163, #650, .T. ) ;
#2148 = CARTESIAN_POINT ( 'NONE',  ( 87.00000000000000000, -7.622732162557277534E-15, 7.500000000000000000 ) ) ;
#2149 = PRODUCT_CONTEXT ( 'NONE', #642, 'mechanical' ) ;
#2150 = AXIS2_PLACEMENT_3D ( 'NONE', #2627, #1648, #1919 ) ;
#2151 = ORIENTED_EDGE ( 'NONE', *, *, #1701, .F. ) ;
#2152 = CARTESIAN_POINT ( 'NONE',  ( -37.00000000000000000, -5.785761963836251101E-15, 7.500000000000000000 ) ) ;
#2153 = CARTESIAN_POINT ( 'NONE',  ( 100.0000000000000000, -6.928842772166554697E-15, 7.500000000000000000 ) ) ;
#2154 = AXIS2_PLACEMENT_3D ( 'NONE', #1655, #1395, #2611 ) ;
#2155 = DIRECTION ( 'NONE',  ( 1.000000000000000000, 0.000000000000000000, 0.000000000000000000 ) ) ;
#2156 = ORIENTED_EDGE ( 'NONE', *, *, #1661, .T. ) ;
#2157 = PLANE ( 'NONE',  #2694 ) ;
#2158 = VECTOR ( 'NONE', #2931, 1000.000000000000000 ) ;
#2159 = VECTOR ( 'NONE', #2309, 1000.000000000000000 ) ;
#2160 = EDGE_LOOP ( 'NONE', ( #1914, #1437, #1156, #159, #2590, #2036 ) ) ;
#2161 = VECTOR ( 'NONE', #710, 1000.000000000000000 ) ;
#2162 = VECTOR ( 'NONE', #1928, 1000.000000000000000 ) ;
#2163 = ORIENTED_EDGE ( 'NONE', *, *, #677, .T. ) ;
#2164 = EDGE_CURVE ( 'NONE', #1964, #2636, #3004, .T. ) ;
#2165 = DIRECTION ( 'NONE',  ( -1.000000000000000000, -2.312964634635742957E-16, 0.000000000000000000 ) ) ;
#2166 = DIRECTION ( 'NONE',  ( -1.000000000000000000, -0.000000000000000000, -0.000000000000000000 ) ) ;
#2167 = LINE ( 'NONE', #1165, #410 ) ;
#2168 = SHAPE_DEFINITION_REPRESENTATION ( #248, #2426 ) ;
#2169 = ORIENTED_EDGE ( 'NONE', *, *, #759, .T. ) ;
#2170 = CARTESIAN_POINT ( 'NONE',  ( 30.00000000000000000, -11.82159041753688200, 0.000000000000000000 ) ) ;
#2171 = CARTESIAN_POINT ( 'NONE',  ( 2.168404344971008868E-16, 0.000000000000000000, 0.000000000000000000 ) ) ;
#2172 = ADVANCED_FACE ( 'NONE', ( #2760 ), #536, .T. ) ;
#2173 = DIRECTION ( 'NONE',  ( 0.000000000000000000, -0.5000000000000000000, -0.8660254037844385966 ) ) ;
#2174 = ORIENTED_EDGE ( 'NONE', *, *, #2945, .F. ) ;
#2175 = CARTESIAN_POINT ( 'NONE',  ( -37.00000000000000000, -5.173438564262574571E-15, 12.49999999999999645 ) ) ;
#2176 = ORIENTED_EDGE ( 'NONE', *, *, #692, .F. ) ;
#2177 = CIRCLE ( 'NONE', #1285, 0.1000000000000000472 ) ;
#2178 = EDGE_LOOP ( 'NONE', ( #1617, #1207 ) ) ;
#2179 = DIRECTION ( 'NONE',  ( 0.000000000000000000, 0.000000000000000000, 1.000000000000000000 ) ) ;
#2180 = UNCERTAINTY_MEASURE_WITH_UNIT (LENGTH_MEASURE( 1.000000000000000082E-05 ), #1496, 'distance_accuracy_value', 'NONE');
#2181 = AXIS2_PLACEMENT_3D ( 'NONE', #2260, #2292, #2229 ) ;
#2182 = DIRECTION ( 'NONE',  ( 1.000000000000000000, 0.000000000000000000, 0.000000000000000000 ) ) ;
#2183 = LINE ( 'NONE', #1440, #1814 ) ;
#2184 = CONTEXT_DEPENDENT_SHAPE_REPRESENTATION ( #459, #1973 ) ;
#2185 = EDGE_CURVE ( 'NONE', #1365, #3117, #289, .T. ) ;
#2186 = FILL_AREA_STYLE_COLOUR ( '', #2966 ) ;
#2187 = CARTESIAN_POINT ( 'NONE',  ( 0.000000000000000000, 0.000000000000000000, 0.000000000000000000 ) ) ;
#2188 = EDGE_CURVE ( 'NONE', #779, #1561, #282, .T. ) ;
#2189 = LINE ( 'NONE', #1733, #2934 ) ;
#2190 = CARTESIAN_POINT ( 'NONE',  ( 37.99089481476347174, 1.130332597043749665, 16.42900728359811424 ) ) ;
#2191 = EDGE_CURVE ( 'NONE', #1866, #1415, #3084, .T. ) ;
#2192 = ORIENTED_EDGE ( 'NONE', *, *, #1061, .F. ) ;
#2193 = EDGE_CURVE ( 'NONE', #2689, #1866, #238, .T. ) ;
#2194 = SURFACE_SIDE_STYLE ('',( #1004 ) ) ;
#2195 = ORIENTED_EDGE ( 'NONE', *, *, #2193, .F. ) ;
#2196 = CARTESIAN_POINT ( 'NONE',  ( 1.040000000000000036, -0.5773502691896253980, 1.000000000000000000 ) ) ;
#2197 = AXIS2_PLACEMENT_3D ( 'NONE', #1284, #1299, #407 ) ;
#2198 = DIRECTION ( 'NONE',  ( 1.000000000000000000, 0.000000000000000000, -0.000000000000000000 ) ) ;
#2199 = FACE_OUTER_BOUND ( 'NONE', #3055, .T. ) ;
#2200 = APPLICATION_PROTOCOL_DEFINITION ( 'draft international standard', 'automotive_design', 1998, #133 ) ;
#2201 = DIRECTION ( 'NONE',  ( 2.312964634635742957E-16, -1.000000000000000000, 0.000000000000000000 ) ) ;
#2202 = VECTOR ( 'NONE', #3183, 1000.000000000000000 ) ;
#2203 =( LENGTH_UNIT ( ) NAMED_UNIT ( * ) SI_UNIT ( .MILLI., .METRE. ) );
#2204 = DIRECTION ( 'NONE',  ( 0.000000000000000000, 0.000000000000000000, -1.000000000000000000 ) ) ;
#2205 = LINE ( 'NONE', #2949, #630 ) ;
#2206 = AXIS2_PLACEMENT_3D ( 'NONE', #3070, #345, #908 ) ;
#2207 = ORIENTED_EDGE ( 'NONE', *, *, #2440, .F. ) ;
#2208 = ORIENTED_EDGE ( 'NONE', *, *, #1634, .F. ) ;
#2209 = AXIS2_PLACEMENT_3D ( 'NONE', #2961, #2715, #2204 ) ;
#2210 = MECHANICAL_DESIGN_GEOMETRIC_PRESENTATION_REPRESENTATION (  '', ( #2723 ), #3038 ) ;
#2211 = EDGE_CURVE ( 'NONE', #3095, #1890, #35, .T. ) ;
#2212 = CARTESIAN_POINT ( 'NONE',  ( 87.00000000000000000, -7.622732162557277534E-15, 7.500000000000000000 ) ) ;
#2213 = AXIS2_PLACEMENT_3D ( 'NONE', #1277, #1494, #1294 ) ;
#2214 = CIRCLE ( 'NONE', #2938, 1.499999999999994449 ) ;
#2215 = DIRECTION ( 'NONE',  ( -2.312964634635742957E-16, 1.000000000000000000, 0.000000000000000000 ) ) ;
#2216 = CARTESIAN_POINT ( 'NONE',  ( 3.469446951953614189E-15, -15.00000000000000355, 0.000000000000000000 ) ) ;
#2217 = DIRECTION ( 'NONE',  ( 1.000000000000000000, 2.312964634635742957E-16, 0.000000000000000000 ) ) ;
#2218 = APPLICATION_PROTOCOL_DEFINITION ( 'draft international standard', 'automotive_design', 1998, #1577 ) ;
#2219 = AXIS2_PLACEMENT_3D ( 'NONE', #934, #3167, #1666 ) ;
#2220 = AXIS2_PLACEMENT_3D ( 'NONE', #755, #1727, #2243 ) ;
#2221 = DIRECTION ( 'NONE',  ( 0.000000000000000000, 0.000000000000000000, -1.000000000000000000 ) ) ;
#2222 = SURFACE_STYLE_USAGE ( .BOTH. , #1974 ) ;
#2223 = DIRECTION ( 'NONE',  ( 1.000000000000000000, 0.000000000000000000, -0.000000000000000000 ) ) ;
#2224 = DIRECTION ( 'NONE',  ( 0.000000000000000000, 0.000000000000000000, -1.000000000000000000 ) ) ;
#2225 = ORIENTED_EDGE ( 'NONE', *, *, #2619, .T. ) ;
#2226 = ORIENTED_EDGE ( 'NONE', *, *, #1424, .T. ) ;
#2227 = DIRECTION ( 'NONE',  ( -1.000000000000000000, -0.000000000000000000, -0.000000000000000000 ) ) ;
#2228 = CARTESIAN_POINT ( 'NONE',  ( 37.41786025882474576, -7.616137346557303354E-15, 12.50000000000000000 ) ) ;
#2229 = DIRECTION ( 'NONE',  ( -2.312964634635742957E-16, 1.000000000000000000, 0.000000000000000000 ) ) ;
#2230 = ADVANCED_FACE ( 'NONE', ( #2294 ), #50, .T. ) ;
#2231 = CONTEXT_DEPENDENT_SHAPE_REPRESENTATION ( #1691, #278 ) ;
#2232 = ADVANCED_FACE ( 'NONE', ( #2234 ), #2880, .F. ) ;
#2233 = PRODUCT_RELATED_PRODUCT_CATEGORY ( 'part', '', ( #2617 ) ) ;
#2234 = FACE_OUTER_BOUND ( 'NONE', #1835, .T. ) ;
#2235 = CIRCLE ( 'NONE', #2020, 3.351416843938785028 ) ;
#2236 = CARTESIAN_POINT ( 'NONE',  ( 1.750000000000000000, 0.000000000000000000, 0.000000000000000000 ) ) ;
#2237 = PRODUCT ( 'socket button head screw_iso_ISO 7380 - M3 x 6 - 6N', 'socket button head screw_iso_ISO 7380 - M3 x 6 - 6N', '', ( #2149 ) ) ;
#2238 = EDGE_LOOP ( 'NONE', ( #245, #2922, #794, #2011 ) ) ;
#2239 = LINE ( 'NONE', #2441, #116 ) ;
#2240 = FACE_OUTER_BOUND ( 'NONE', #3148, .T. ) ;
#2241 = ORIENTED_EDGE ( 'NONE', *, *, #2759, .T. ) ;
#2242 = ORIENTED_EDGE ( 'NONE', *, *, #1286, .F. ) ;
#2243 = DIRECTION ( 'NONE',  ( 0.000000000000000000, 0.000000000000000000, -1.000000000000000000 ) ) ;
#2244 = CARTESIAN_POINT ( 'NONE',  ( 7.650000000000000355, 1.493456771560197319E-16, -1.219500000000000028 ) ) ;
#2245 = CARTESIAN_POINT ( 'NONE',  ( 36.58213974117523293, -6.323013916343274967E-15, 12.50000000000000178 ) ) ;
#2246 = APPLICATION_PROTOCOL_DEFINITION ( 'draft international standard', 'automotive_design', 1998, #1344 ) ;
#2247 = DIRECTION ( 'NONE',  ( 1.000000000000000000, 2.312964634635742957E-16, 0.000000000000000000 ) ) ;
#2248 = EDGE_CURVE ( 'NONE', #1561, #779, #1900, .T. ) ;
#2249 = DIRECTION ( 'NONE',  ( 1.000000000000000000, 2.312964634635742957E-16, 0.000000000000000000 ) ) ;
#2250=STYLED_ITEM('',(#3271),#2105);
#2251 = ORIENTED_EDGE ( 'NONE', *, *, #147, .F. ) ;
#2252 = DIRECTION ( 'NONE',  ( -1.000000000000000000, -2.312964634635742957E-16, 0.000000000000000000 ) ) ;
#2253 = CARTESIAN_POINT ( 'NONE',  ( 52.00000000000000711, -3.708099243547825274, 20.99999999999999645 ) ) ;
#2254 = FACE_OUTER_BOUND ( 'NONE', #581, .T. ) ;
#2255 = ORIENTED_EDGE ( 'NONE', *, *, #1149, .F. ) ;
#2256 = EDGE_LOOP ( 'NONE', ( #661, #870, #2226, #2608, #3153, #932 ) ) ;
#2257 = PRODUCT ( 'Spindle Shaft Rod', 'Spindle Shaft Rod', '', ( #253 ) ) ;
#2258 = FACE_OUTER_BOUND ( 'NONE', #2754, .T. ) ;
#2259 = CARTESIAN_POINT ( 'NONE',  ( 37.09819064725438409, -1.500059831078487171, 16.37410956135322948 ) ) ;
#2260 = CARTESIAN_POINT ( 'NONE',  ( 87.00000000000000000, -7.622732162557277534E-15, 7.500000000000000000 ) ) ;
#2261 = CIRCLE ( 'NONE', #2459, 8.999999999999989342 ) ;
#2262 = EDGE_CURVE ( 'NONE', #359, #3085, #255, .T. ) ;
#2263 = LINE ( 'NONE', #1131, #2668 ) ;
#2264 = AXIS2_PLACEMENT_3D ( 'NONE', #3080, #3112, #1372 ) ;
#2265 = VECTOR ( 'NONE', #2384, 1000.000000000000000 ) ;
#2266 = ORIENTED_EDGE ( 'NONE', *, *, #1510, .F. ) ;
#2267 = ADVANCED_BREP_SHAPE_REPRESENTATION ( '', ( #1054, #2878 ), #603 ) ;
#2268 = LINE ( 'NONE', #1019, #1703 ) ;
#2269 = FACE_OUTER_BOUND ( 'NONE', #1629, .T. ) ;
#2270 = ADVANCED_FACE ( 'NONE', ( #1761 ), #2496, .F. ) ;
#2271 = DIRECTION ( 'NONE',  ( 0.000000000000000000, 0.000000000000000000, 1.000000000000000000 ) ) ;
#2272 = ORIENTED_EDGE ( 'NONE', *, *, #2442, .T. ) ;
#2273 = B_SPLINE_CURVE_WITH_KNOTS ( 'NONE', 3,
 ( #1787, #2773, #2806, #553, #2493, #73, #1041, #1542, #3002, #992, #1255, #2259, #1996, #2510, #16, #1774, #2045, #2757, #533, #287, #1847, #107, #366, #1351 ),
 .UNSPECIFIED., .F., .F.,
 ( 4, 2, 2, 2, 2, 2, 2, 2, 2, 2, 2, 4 ),
 ( 0.004697885398315485364, 0.005284974574641448583, 0.005872063750967410935, 0.006165608339130399483, 0.006459152927293387164, 0.007046242103619364261, 0.007339786691782353677, 0.007633331279945342225, 0.007926875868108331641, 0.008220420456271318455, 0.008807509632597297286, 0.009394598808923274383 ),
 .UNSPECIFIED. ) ;
#2274 = CARTESIAN_POINT ( 'NONE',  ( 38.49999999999999289, -7.622732162557277534E-15, 16.49999999999999289 ) ) ;
#2275 = FACE_OUTER_BOUND ( 'NONE', #2577, .T. ) ;
#2276 = CARTESIAN_POINT ( 'NONE',  ( 37.00000000000000000, 1.474514954580286030E-14, 13.99999999999999822 ) ) ;
#2277 = DIRECTION ( 'NONE',  ( 0.000000000000000000, 0.000000000000000000, -1.000000000000000000 ) ) ;
#2278 = SURFACE_STYLE_FILL_AREA ( #2972 ) ;
#2279 = FILL_AREA_STYLE ('',( #2545 ) ) ;
#2280 = ORIENTED_EDGE ( 'NONE', *, *, #772, .F. ) ;
#2281 = AXIS2_PLACEMENT_3D ( 'NONE', #68, #3099, #865 ) ;
#2282 = AXIS2_PLACEMENT_3D ( 'NONE', #1507, #1788, #1760 ) ;
#2283 = CARTESIAN_POINT ( 'NONE',  ( 36.24410157368015462, 1.310477515366009760, 16.40440676504734085 ) ) ;
#2284 = FACE_OUTER_BOUND ( 'NONE', #1293, .T. ) ;
#2285 = PRODUCT ( 'anvil', 'anvil', '', ( #437 ) ) ;
#2286 = DIRECTION ( 'NONE',  ( 0.000000000000000000, -1.000000000000000000, 0.000000000000000000 ) ) ;
#2287 = ADVANCED_FACE ( 'NONE', ( #2747 ), #269, .F. ) ;
#2288 =( NAMED_UNIT ( * ) PLANE_ANGLE_UNIT ( ) SI_UNIT ( $, .RADIAN. ) );
#2289 = ORIENTED_EDGE ( 'NONE', *, *, #2129, .F. ) ;
#2290 = LINE ( 'NONE', #1786, #2882 ) ;
#2291 = CARTESIAN_POINT ( 'NONE',  ( 100.0000000000000000, -6.928842772166554697E-15, 7.500000000000000000 ) ) ;
#2292 = DIRECTION ( 'NONE',  ( 1.000000000000000000, 2.312964634635742957E-16, 0.000000000000000000 ) ) ;
#2293 = ORIENTED_EDGE ( 'NONE', *, *, #2906, .T. ) ;
#2294 = FACE_OUTER_BOUND ( 'NONE', #1832, .T. ) ;
#2295 = CARTESIAN_POINT ( 'NONE',  ( 27.00000000000000000, 1.133017633246824688E-14, -1.499999999999994449 ) ) ;
#2296 = VECTOR ( 'NONE', #393, 1000.000000000000000 ) ;
#2297 = ORIENTED_EDGE ( 'NONE', *, *, #2864, .T. ) ;
#2298 = EDGE_CURVE ( 'NONE', #137, #1084, #2263, .T. ) ;
#2299 = FACE_OUTER_BOUND ( 'NONE', #1011, .T. ) ;
#2300 = CARTESIAN_POINT ( 'NONE',  ( -41.99999999999999289, -6.449497959004950529E-15, 0.000000000000000000 ) ) ;
#2301 = ORIENTED_EDGE ( 'NONE', *, *, #2921, .T. ) ;
#2302 = AXIS2_PLACEMENT_3D ( 'NONE', #2657, #433, #2414 ) ;
#2303 = ORIENTED_EDGE ( 'NONE', *, *, #3182, .T. ) ;
#2304 = DIRECTION ( 'NONE',  ( 2.312964634635742957E-16, -1.000000000000000000, 0.000000000000000000 ) ) ;
#2305 = PLANE ( 'NONE',  #1535 ) ;
#2306 = DIRECTION ( 'NONE',  ( -1.000000000000000000, -0.000000000000000000, -0.000000000000000000 ) ) ;
#2307 = ORIENTED_EDGE ( 'NONE', *, *, #931, .F. ) ;
#2308 = EDGE_CURVE ( 'NONE', #628, #2825, #1218, .T. ) ;
#2309 = DIRECTION ( 'NONE',  ( 1.000000000000000000, -0.000000000000000000, -0.000000000000000000 ) ) ;
#2310 = MECHANICAL_DESIGN_GEOMETRIC_PRESENTATION_REPRESENTATION (  '', ( #489 ), #1420 ) ;
#2311 = ORIENTED_EDGE ( 'NONE', *, *, #517, .T. ) ;
#2312 = AXIS2_PLACEMENT_3D ( 'NONE', #1672, #3142, #1364 ) ;
#2313 = CARTESIAN_POINT ( 'NONE',  ( 35.75000000000000000, 1.489823039569627924E-14, 12.99999999999999822 ) ) ;
#2314 = AXIS2_PLACEMENT_3D ( 'NONE', #1268, #2654, #3180 ) ;
#2315 = AXIS2_PLACEMENT_3D ( 'NONE', #1995, #532, #2726 ) ;
#2316 = DIRECTION ( 'NONE',  ( 1.000000000000000000, -0.000000000000000000, -0.000000000000000000 ) ) ;
#2317 = EDGE_LOOP ( 'NONE', ( #75, #131, #162 ) ) ;
#2318 = DIRECTION ( 'NONE',  ( -0.000000000000000000, -0.5000000000000000000, 0.8660254037844385966 ) ) ;
#2319 = CARTESIAN_POINT ( 'NONE',  ( -5.000000000000000000, -6.316519372592878167E-15, 12.50000000000000000 ) ) ;
#2320 = ORIENTED_EDGE ( 'NONE', *, *, #721, .F. ) ;
#2321 = CARTESIAN_POINT ( 'NONE',  ( 100.0000000000000000, -6.928842772166554697E-15, 7.500000000000000000 ) ) ;
#2322 = EDGE_CURVE ( 'NONE', #163, #1134, #1839, .T. ) ;
#2323 = CARTESIAN_POINT ( 'NONE',  ( -30.00000000000000000, -3.673940397442059178E-15, 15.00000000000000000 ) ) ;
#2324 = PRODUCT_DEFINITION ( 'UNKNOWN', '', #2831, #1422 ) ;
#2325 = ORIENTED_EDGE ( 'NONE', *, *, #692, .T. ) ;
#2326 = EDGE_CURVE ( 'NONE', #137, #106, #115, .T. ) ;
#2327 = DIRECTION ( 'NONE',  ( 1.000000000000000000, 2.312964634635742957E-16, 0.000000000000000000 ) ) ;
#2328 = FACE_OUTER_BOUND ( 'NONE', #2379, .T. ) ;
#2329 = VECTOR ( 'NONE', #1295, 1000.000000000000000 ) ;
#2330 = AXIS2_PLACEMENT_3D ( 'NONE', #520, #1256, #2015 ) ;
#2331 = LINE ( 'NONE', #158, #2670 ) ;
#2332 = ORIENTED_EDGE ( 'NONE', *, *, #2110, .F. ) ;
#2333 = DIRECTION ( 'NONE',  ( -0.000000000000000000, 0.5000000000000003331, -0.8660254037844383745 ) ) ;
#2334 = DIRECTION ( 'NONE',  ( 1.000000000000000000, 0.000000000000000000, 0.000000000000000000 ) ) ;
#2335 = EDGE_LOOP ( 'NONE', ( #2354, #498 ) ) ;
#2336 = PLANE ( 'NONE',  #1746 ) ;
#2337 = CARTESIAN_POINT ( 'NONE',  ( 1.040000000000000036, 0.5773502691896263972, 1.000000000000000000 ) ) ;
#2338 = APPLICATION_PROTOCOL_DEFINITION ( 'draft international standard', 'automotive_design', 1998, #3029 ) ;
#2339 = ORIENTED_EDGE ( 'NONE', *, *, #559, .T. ) ;
#2340 = EDGE_CURVE ( 'NONE', #1599, #1482, #3041, .T. ) ;
#2341 = ORIENTED_EDGE ( 'NONE', *, *, #2852, .T. ) ;
#2342 = DIRECTION ( 'NONE',  ( -0.000000000000000000, 1.000000000000000000, -0.000000000000000000 ) ) ;
#2343 = EDGE_CURVE ( 'NONE', #2077, #415, #1167, .T. ) ;
#2344 = AXIS2_PLACEMENT_3D ( 'NONE', #2738, #1251, #244 ) ;
#2345 = FACE_OUTER_BOUND ( 'NONE', #2256, .T. ) ;
#2346 = VERTEX_POINT ( 'NONE', #1885 ) ;
#2347 = AXIS2_PLACEMENT_3D ( 'NONE', #1438, #2431, #200 ) ;
#2348 = VERTEX_POINT ( 'NONE', #2351 ) ;
#2349 = LINE ( 'NONE', #580, #2265 ) ;
#2350 = VERTEX_POINT ( 'NONE', #132 ) ;
#2351 = CARTESIAN_POINT ( 'NONE',  ( 7.650000000000000355, 1.665213485140613626E-16, -1.219500000000000028 ) ) ;
#2352 = CARTESIAN_POINT ( 'NONE',  ( 0.000000000000000000, 0.000000000000000000, 0.000000000000000000 ) ) ;
#2353 = SHAPE_REPRESENTATION_RELATIONSHIP ( 'NONE' , 'NONE' ,  #524, #824 ) ;
#2354 = ORIENTED_EDGE ( 'NONE', *, *, #1886, .T. ) ;
#2355 = VERTEX_POINT ( 'NONE', #111 ) ;
#2356 = CARTESIAN_POINT ( 'NONE',  ( -26.99999999999999645, -7.500000000000007105, 7.500000000000000000 ) ) ;
#2357 = AXIS2_PLACEMENT_3D ( 'NONE', #1231, #3220, #997 ) ;
#2358 = FACE_OUTER_BOUND ( 'NONE', #1102, .T. ) ;
#2359 = AXIS2_PLACEMENT_3D ( 'NONE', #1820, #1404, #948 ) ;
#2360 = VECTOR ( 'NONE', #3193, 1000.000000000000000 ) ;
#2361 = EDGE_CURVE ( 'NONE', #1803, #2769, #493, .T. ) ;
#2362 = CARTESIAN_POINT ( 'NONE',  ( 3.469446951953614189E-15, -15.00000000000000355, 15.00000000000000000 ) ) ;
#2363 = ORIENTED_EDGE ( 'NONE', *, *, #2164, .F. ) ;
#2364 = UNCERTAINTY_MEASURE_WITH_UNIT (LENGTH_MEASURE( 1.000000000000000082E-05 ), #189, 'distance_accuracy_value', 'NONE');
#2365 = CARTESIAN_POINT ( 'NONE',  ( 36.33339417452628339, 1.347339434735567609, 16.39865934157270289 ) ) ;
#2366 = COLOUR_RGB ( '',1.000000000000000000, 0.9490196078431372140, 0.9098039215686274384 ) ;
#2367 = EDGE_LOOP ( 'NONE', ( #1377, #2297, #678, #2369 ) ) ;
#2368 = DIRECTION ( 'NONE',  ( 1.000000000000000000, 0.000000000000000000, 0.000000000000000000 ) ) ;
#2369 = ORIENTED_EDGE ( 'NONE', *, *, #1243, .F. ) ;
#2370 = DIRECTION ( 'NONE',  ( 0.000000000000000000, 0.000000000000000000, -1.000000000000000000 ) ) ;
#2371 = CARTESIAN_POINT ( 'NONE',  ( 155.0000000000000284, -6.928842772166554697E-15, 12.50000000000000000 ) ) ;
#2372 = DIRECTION ( 'NONE',  ( 0.000000000000000000, 0.000000000000000000, 1.000000000000000000 ) ) ;
#2373 = VERTEX_POINT ( 'NONE', #848 ) ;
#2374 = EDGE_LOOP ( 'NONE', ( #1862, #2866, #1072, #1548, #1058 ) ) ;
#2375 = CYLINDRICAL_SURFACE ( 'NONE', #2596, 4.999999999999999112 ) ;
#2376 = FACE_BOUND ( 'NONE', #2803, .T. ) ;
#2377 = DIRECTION ( 'NONE',  ( 1.000000000000000000, 0.000000000000000000, 0.000000000000000000 ) ) ;
#2378 = CARTESIAN_POINT ( 'NONE',  ( 1.040000000000000036, 0.000000000000000000, -1.000000000000000000 ) ) ;
#2379 = EDGE_LOOP ( 'NONE', ( #324, #1755, #1343, #1665, #529, #1012, #2242, #2620 ) ) ;
#2380 = AXIS2_PLACEMENT_3D ( 'NONE', #2434, #2944, #484 ) ;
#2381 = DIRECTION ( 'NONE',  ( 0.000000000000000000, 0.000000000000000000, -1.000000000000000000 ) ) ;
#2382 = EDGE_CURVE ( 'NONE', #548, #516, #2982, .T. ) ;
#2383 = ORIENTED_EDGE ( 'NONE', *, *, #151, .T. ) ;
#2384 = DIRECTION ( 'NONE',  ( -1.000000000000000000, 0.000000000000000000, 0.000000000000000000 ) ) ;
#2385 = ORIENTED_EDGE ( 'NONE', *, *, #3, .F. ) ;
#2386 = FACE_OUTER_BOUND ( 'NONE', #690, .T. ) ;
#2387 = FACE_OUTER_BOUND ( 'NONE', #1468, .T. ) ;
#2388 = EDGE_LOOP ( 'NONE', ( #2855, #1658, #2980, #183 ) ) ;
#2389 = DIRECTION ( 'NONE',  ( -1.000000000000000000, -0.000000000000000000, -0.000000000000000000 ) ) ;
#2390 = PRODUCT_DEFINITION_SHAPE ( 'NONE', 'NONE',  #3229 ) ;
#2391 = CARTESIAN_POINT ( 'NONE',  ( -5.000000000000000000, -6.928842772166554697E-15, 2.499999999999999556 ) ) ;
#2392 = ADVANCED_FACE ( 'NONE', ( #2869, #1340 ), #2336, .F. ) ;
#2393 = CYLINDRICAL_SURFACE ( 'NONE', #2512, 5.000000000000000888 ) ;
#2394 = VERTEX_POINT ( 'NONE', #863 ) ;
#2395 = AXIS2_PLACEMENT_3D ( 'NONE', #1736, #209, #1269 ) ;
#2396 = PLANE ( 'NONE',  #1863 ) ;
#2397 = VERTEX_POINT ( 'NONE', #1110 ) ;
#2398 = ORIENTED_EDGE ( 'NONE', *, *, #927, .T. ) ;
#2399 = CYLINDRICAL_SURFACE ( 'NONE', #53, 5.000000000000000888 ) ;
#2400 = DIRECTION ( 'NONE',  ( 1.000000000000000000, -0.000000000000000000, -0.000000000000000000 ) ) ;
#2401 = DIRECTION ( 'NONE',  ( 0.000000000000000000, 0.000000000000000000, 1.000000000000000000 ) ) ;
#2402 = ADVANCED_FACE ( 'NONE', ( #338 ), #646, .F. ) ;
#2403 = ORIENTED_EDGE ( 'NONE', *, *, #2248, .F. ) ;
#2404 = DIRECTION ( 'NONE',  ( 1.000000000000000000, 0.000000000000000000, 0.000000000000000000 ) ) ;
#2405 = SURFACE_STYLE_FILL_AREA ( #3122 ) ;
#2406 = CIRCLE ( 'NONE', #2051, 11.00000000000000355 ) ;
#2407 = CARTESIAN_POINT ( 'NONE',  ( 1.269999999999999796, 0.000000000000000000, 2.849999999999999645 ) ) ;
#2408 = ORIENTED_EDGE ( 'NONE', *, *, #1580, .T. ) ;
#2409 = DIRECTION ( 'NONE',  ( 1.000000000000000000, 2.312964634635742957E-16, 0.000000000000000000 ) ) ;
#2410 = ORIENTED_EDGE ( 'NONE', *, *, #1206, .F. ) ;
#2411 = CARTESIAN_POINT ( 'NONE',  ( -26.99999999999999645, 7.499999999999992006, 7.500000000000000888 ) ) ;
#2412 = CIRCLE ( 'NONE', #341, 14.00000000000000000 ) ;
#2413 = ORIENTED_EDGE ( 'NONE', *, *, #3060, .T. ) ;
#2414 = DIRECTION ( 'NONE',  ( 0.000000000000000000, 0.000000000000000000, -1.000000000000000000 ) ) ;
#2415 = DIRECTION ( 'NONE',  ( -1.000000000000000000, -0.000000000000000000, -0.000000000000000000 ) ) ;
#2416 = DIRECTION ( 'NONE',  ( -2.478176394252581634E-16, 1.000000000000000000, 0.000000000000000000 ) ) ;
#2417 = FILL_AREA_STYLE_COLOUR ( '', #2859 ) ;
#2418 = EDGE_CURVE ( 'NONE', #1829, #1561, #1077, .T. ) ;
#2419 = DIRECTION ( 'NONE',  ( -0.000000000000000000, 0.000000000000000000, 1.000000000000000000 ) ) ;
#2420 = PRODUCT_RELATED_PRODUCT_CATEGORY ( 'part', '', ( #2716 ) ) ;
#2421 = FILL_AREA_STYLE_COLOUR ( '', #705 ) ;
#2422 = EDGE_CURVE ( 'NONE', #479, #2394, #2513, .T. ) ;
#2423 = UNCERTAINTY_MEASURE_WITH_UNIT (LENGTH_MEASURE( 1.000000000000000082E-05 ), #1413, 'distance_accuracy_value', 'NONE');
#2424 = CARTESIAN_POINT ( 'NONE',  ( 3.469446951953614189E-15, -15.00000000000000355, 15.00000000000000000 ) ) ;
#2425 = DIRECTION ( 'NONE',  ( 1.000000000000000000, 0.000000000000000000, 0.000000000000000000 ) ) ;
#2426 = SHAPE_REPRESENTATION ( 'MAS-165', ( #1487, #1591, #1485, #70, #1907, #754, #3145, #1751 ), #1754 ) ;
#2427 = VERTEX_POINT ( 'NONE', #597 ) ;
#2428 = SURFACE_SIDE_STYLE ('',( #182 ) ) ;
#2429 = CIRCLE ( 'NONE', #1021, 41.99999999999999289 ) ;
#2430 = VERTEX_POINT ( 'NONE', #1624 ) ;
#2431 = DIRECTION ( 'NONE',  ( 0.000000000000000000, 0.8660254037844384856, -0.5000000000000004441 ) ) ;
#2432 = AXIS2_PLACEMENT_3D ( 'NONE', #2276, #1557, #2541 ) ;
#2433 = CARTESIAN_POINT ( 'NONE',  ( 27.00000000000000000, 6.704247063196759979E-15, 7.500000000000000000 ) ) ;
#2434 = CARTESIAN_POINT ( 'NONE',  ( 37.00000000000000000, 1.474514954580286030E-14, 12.99999999999999822 ) ) ;
#2435 = ITEM_DEFINED_TRANSFORMATION ( 'NONE', 'NONE', #1751,  #2878 ) ;
#2436 = DIRECTION ( 'NONE',  ( 0.000000000000000000, 0.000000000000000000, -1.000000000000000000 ) ) ;
#2437 = DIRECTION ( 'NONE',  ( 0.000000000000000000, 0.000000000000000000, 1.000000000000000000 ) ) ;
#2438 = AXIS2_PLACEMENT_3D ( 'NONE', #2682, #3170, #454 ) ;
#2439 = APPLICATION_PROTOCOL_DEFINITION ( 'draft international standard', 'automotive_design', 1998, #1516 ) ;
#2440 = EDGE_CURVE ( 'NONE', #391, #2818, #1592, .T. ) ;
#2441 = CARTESIAN_POINT ( 'NONE',  ( 27.00000000000000000, 3.708099243547847479, 20.99999999999999645 ) ) ;
#2442 = EDGE_CURVE ( 'NONE', #2769, #1803, #173, .T. ) ;
#2443 = DIRECTION ( 'NONE',  ( 0.000000000000000000, 0.000000000000000000, -1.000000000000000000 ) ) ;
#2444 = ORIENTED_EDGE ( 'NONE', *, *, #866, .T. ) ;
#2445 = CYLINDRICAL_SURFACE ( 'NONE', #229, 1.499999999999999556 ) ;
#2446 = AXIS2_PLACEMENT_3D ( 'NONE', #2785, #55, #2058 ) ;
#2447 = ORIENTED_EDGE ( 'NONE', *, *, #2185, .T. ) ;
#2448 = CARTESIAN_POINT ( 'NONE',  ( 38.25000000000000000, 1.474514954580286030E-14, 13.99999999999999822 ) ) ;
#2449 = DIRECTION ( 'NONE',  ( 0.000000000000000000, 0.000000000000000000, 1.000000000000000000 ) ) ;
#2450 = CARTESIAN_POINT ( 'NONE',  ( 27.00000000000000000, 6.704247063196759979E-15, 7.500000000000000000 ) ) ;
#2451 = DIRECTION ( 'NONE',  ( -0.000000000000000000, -0.000000000000000000, -1.000000000000000000 ) ) ;
#2452 = ITEM_DEFINED_TRANSFORMATION ( 'NONE', 'NONE', #1907,  #2878 ) ;
#2453 = FACE_OUTER_BOUND ( 'NONE', #2238, .T. ) ;
#2454 = CIRCLE ( 'NONE', #2042, 8.000000000000000000 ) ;
#2455 = FILL_AREA_STYLE ('',( #1462 ) ) ;
#2456 = ADVANCED_BREP_SHAPE_REPRESENTATION ( '', ( #3178, #2878 ), #2989 ) ;
#2457 = CARTESIAN_POINT ( 'NONE',  ( -5.000000000000000000, -6.928842772166554697E-15, 7.500000000000000000 ) ) ;
#2458 = CARTESIAN_POINT ( 'NONE',  ( 2.168404344971008868E-16, -0.5773502691896253980, 1.000000000000000000 ) ) ;
#2459 = AXIS2_PLACEMENT_3D ( 'NONE', #1201, #190, #1958 ) ;
#2460 = ADVANCED_FACE ( 'NONE', ( #353 ), #1867, .T. ) ;
#2461 = ORIENTED_EDGE ( 'NONE', *, *, #615, .F. ) ;
#2462 = ORIENTED_EDGE ( 'NONE', *, *, #184, .T. ) ;
#2463 = PLANE ( 'NONE',  #215 ) ;
#2464 = AXIS2_PLACEMENT_3D ( 'NONE', #2820, #90, #1323 ) ;
#2465 = AXIS2_PLACEMENT_3D ( 'NONE', #2424, #2995, #1768 ) ;
#2466 = FACE_BOUND ( 'NONE', #858, .T. ) ;
#2467 = CARTESIAN_POINT ( 'NONE',  ( 1.040000000000000036, -0.5773502691896253980, 1.000000000000000000 ) ) ;
#2468 = DIRECTION ( 'NONE',  ( -0.000000000000000000, 0.000000000000000000, -1.000000000000000000 ) ) ;
#2469 = SHAPE_DEFINITION_REPRESENTATION ( #907, #514 ) ;
#2470 = CARTESIAN_POINT ( 'NONE',  ( 1.040000000000000036, 0.000000000000000000, 0.000000000000000000 ) ) ;
#2471 = DIRECTION ( 'NONE',  ( -0.000000000000000000, 0.000000000000000000, 1.000000000000000000 ) ) ;
#2472 = ORIENTED_EDGE ( 'NONE', *, *, #3037, .T. ) ;
#2473 = CARTESIAN_POINT ( 'NONE',  ( 70.00000000000032685, -6.928842772166554697E-15, 7.500000000000000000 ) ) ;
#2474 = DIRECTION ( 'NONE',  ( -0.000000000000000000, -0.000000000000000000, 1.000000000000000000 ) ) ;
#2475 = ORIENTED_EDGE ( 'NONE', *, *, #1772, .T. ) ;
#2476 = ORIENTED_EDGE ( 'NONE', *, *, #2714, .T. ) ;
#2477 = EDGE_CURVE ( 'NONE', #1860, #628, #3056, .T. ) ;
#2478 = DIRECTION ( 'NONE',  ( -1.000000000000000000, -0.000000000000000000, -0.000000000000000000 ) ) ;
#2479 = CARTESIAN_POINT ( 'NONE',  ( -998.3826497308103853, 0.000000000000000000, 0.000000000000000000 ) ) ;
#2480 = CARTESIAN_POINT ( 'NONE',  ( 155.0000000000000284, -6.928842772166554697E-15, 15.50000000000000000 ) ) ;
#2481 = APPLICATION_PROTOCOL_DEFINITION ( 'draft international standard', 'automotive_design', 1998, #2801 ) ;
#2482 = CARTESIAN_POINT ( 'NONE',  ( 100.0000000000000000, -6.928842772166554697E-15, 7.500000000000000000 ) ) ;
#2483 = AXIS2_PLACEMENT_3D ( 'NONE', #3222, #34, #48 ) ;
#2484 = DIRECTION ( 'NONE',  ( 2.312964634635742957E-16, -1.000000000000000000, 0.000000000000000000 ) ) ;
#2485 = ORIENTED_EDGE ( 'NONE', *, *, #3208, .F. ) ;
#2486 = CARTESIAN_POINT ( 'NONE',  ( 100.0000000000000000, -6.928842772166554697E-15, 7.500000000000000000 ) ) ;
#2487 = DIRECTION ( 'NONE',  ( -1.000000000000000000, 0.000000000000000000, 0.000000000000000000 ) ) ;
#2488 = CARTESIAN_POINT ( 'NONE',  ( 38.49999999999999289, 1.474514954580286030E-14, 20.99999999999999645 ) ) ;
#2489 = EDGE_CURVE ( 'NONE', #169, #373, #547, .T. ) ;
#2490 = EDGE_LOOP ( 'NONE', ( #2123, #1771, #1856, #1539 ) ) ;
#2491 = ORIENTED_EDGE ( 'NONE', *, *, #721, .T. ) ;
#2492 = CARTESIAN_POINT ( 'NONE',  ( 1.269999999999999796, 2.849999999999999645, 0.000000000000000000 ) ) ;
#2493 = CARTESIAN_POINT ( 'NONE',  ( 35.80050950286611311, -0.9216565616594013521, 16.45376772233409213 ) ) ;
#2494 = CARTESIAN_POINT ( 'NONE',  ( 47.00000000000000000, 1.133017633246824530E-14, 7.500000000000000000 ) ) ;
#2495 = CIRCLE ( 'NONE', #939, 1.250000000000001110 ) ;
#2496 = PLANE ( 'NONE',  #701 ) ;
#2497 = EDGE_CURVE ( 'NONE', #2346, #1904, #1421, .T. ) ;
#2498 = UNCERTAINTY_MEASURE_WITH_UNIT (LENGTH_MEASURE( 1.000000000000000082E-05 ), #1452, 'distance_accuracy_value', 'NONE');
#2499 = CARTESIAN_POINT ( 'NONE',  ( 100.0000000000000000, -6.928842772166554697E-15, 16.50000000000000000 ) ) ;
#2500 = ORIENTED_EDGE ( 'NONE', *, *, #1606, .T. ) ;
#2501 = VECTOR ( 'NONE', #935, 1000.000000000000000 ) ;
#2502 = DIRECTION ( 'NONE',  ( -0.000000000000000000, -0.000000000000000000, 1.000000000000000000 ) ) ;
#2503 = FACE_OUTER_BOUND ( 'NONE', #1795, .T. ) ;
#2504 = ORIENTED_EDGE ( 'NONE', *, *, #337, .F. ) ;
#2505 = ORIENTED_EDGE ( 'NONE', *, *, #220, .F. ) ;
#2506 =( REPRESENTATION_RELATIONSHIP ('NONE','NONE', #2426, #1790 ) REPRESENTATION_RELATIONSHIP_WITH_TRANSFORMATION ( #2452 )SHAPE_REPRESENTATION_RELATIONSHIP( ) );
#2507 = AXIS2_PLACEMENT_3D ( 'NONE', #538, #308, #2484 ) ;
#2508 = PRODUCT_DEFINITION_SHAPE ( 'NONE', 'NONE',  #1264 ) ;
#2509 = DIRECTION ( 'NONE',  ( -1.000000000000000000, -0.000000000000000000, -0.000000000000000000 ) ) ;
#2510 = CARTESIAN_POINT ( 'NONE',  ( 37.38775466693719807, -1.452318184980603721, 16.38206869443958169 ) ) ;
#2511 = DIRECTION ( 'NONE',  ( 0.000000000000000000, 0.000000000000000000, -1.000000000000000000 ) ) ;
#2512 = AXIS2_PLACEMENT_3D ( 'NONE', #674, #2649, #1177 ) ;
#2513 = CIRCLE ( 'NONE', #1265, 5.000000000000000000 ) ;
#2514 = AXIS2_PLACEMENT_3D ( 'NONE', #2457, #1484, #1235 ) ;
#2515 = DIRECTION ( 'NONE',  ( 1.000000000000000000, 2.312964634635742957E-16, 0.000000000000000000 ) ) ;
#2516 = SHAPE_REPRESENTATION_RELATIONSHIP ( 'NONE' , 'NONE' ,  #2591, #1139 ) ;
#2517 = CONICAL_SURFACE ( 'NONE', #2219, 1.219500000000000028, 0.7853981633974487231 ) ;
#2518 = VECTOR ( 'NONE', #2826, 1000.000000000000000 ) ;
#2519 = ORIENTED_EDGE ( 'NONE', *, *, #811, .F. ) ;
#2520 = ADVANCED_FACE ( 'NONE', ( #1454, #963 ), #418, .F. ) ;
#2521 = MECHANICAL_DESIGN_GEOMETRIC_PRESENTATION_REPRESENTATION (  '', ( #1899 ), #3089 ) ;
#2522 = MECHANICAL_DESIGN_GEOMETRIC_PRESENTATION_REPRESENTATION (  '', ( #1650 ), #2623 ) ;
#2523 = CARTESIAN_POINT ( 'NONE',  ( 36.07902659818448399, 1.200345445641991970, 16.42070378373879080 ) ) ;
#2524 = LINE ( 'NONE', #2300, #2919 ) ;
#2525 = LINE ( 'NONE', #1191, #1698 ) ;
#2526 = ORIENTED_EDGE ( 'NONE', *, *, #575, .F. ) ;
#2527 = DIRECTION ( 'NONE',  ( -0.000000000000000000, -0.000000000000000000, 1.000000000000000000 ) ) ;
#2528 = ADVANCED_FACE ( 'NONE', ( #1183 ), #2517, .T. ) ;
#2529 = CARTESIAN_POINT ( 'NONE',  ( 30.00000000000000000, 7.398136453587482028E-15, 7.500000000000000000 ) ) ;
#2530 = PLANE ( 'NONE',  #2181 ) ;
#2531 = ORIENTED_EDGE ( 'NONE', *, *, #2147, .F. ) ;
#2532 = LINE ( 'NONE', #1810, #2844 ) ;
#2533 = ORIENTED_EDGE ( 'NONE', *, *, #2489, .F. ) ;
#2534 = CARTESIAN_POINT ( 'NONE',  ( 36.90254329834230873, 1.500037116461215625, 16.37411340082286770 ) ) ;
#2535 = CARTESIAN_POINT ( 'NONE',  ( 0.000000000000000000, 0.000000000000000000, 0.000000000000000000 ) ) ;
#2536 = EDGE_CURVE ( 'NONE', #56, #1829, #2925, .T. ) ;
#2537 = ORIENTED_EDGE ( 'NONE', *, *, #731, .T. ) ;
#2538 = EDGE_LOOP ( 'NONE', ( #3179, #43 ) ) ;
#2539 = CARTESIAN_POINT ( 'NONE',  ( 37.00000000000000000, 1.474514954580286030E-14, 12.99999999999999822 ) ) ;
#2540 = DIRECTION ( 'NONE',  ( 0.000000000000000000, 0.000000000000000000, 1.000000000000000000 ) ) ;
#2541 = DIRECTION ( 'NONE',  ( 1.000000000000000000, 0.000000000000000000, 0.000000000000000000 ) ) ;
#2542 = ORIENTED_EDGE ( 'NONE', *, *, #2477, .T. ) ;
#2543 = DIRECTION ( 'NONE',  ( 0.000000000000000000, 0.000000000000000000, -1.000000000000000000 ) ) ;
#2544 = CARTESIAN_POINT ( 'NONE',  ( 27.00000000000000000, 3.708099243547847479, 20.99999999999999645 ) ) ;
#2545 = FILL_AREA_STYLE_COLOUR ( '', #2733 ) ;
#2546 = ORIENTED_EDGE ( 'NONE', *, *, #748, .F. ) ;
#2547 = DIRECTION ( 'NONE',  ( -0.000000000000000000, -0.000000000000000000, 1.000000000000000000 ) ) ;
#2548 =( NAMED_UNIT ( * ) SI_UNIT ( $, .STERADIAN. ) SOLID_ANGLE_UNIT ( ) );
#2549 = DIRECTION ( 'NONE',  ( 0.000000000000000000, -1.000000000000000000, 0.000000000000000000 ) ) ;
#2550 = VECTOR ( 'NONE', #786, 999.9999999999998863 ) ;
#2551 = ORIENTED_EDGE ( 'NONE', *, *, #1793, .T. ) ;
#2552 = ADVANCED_FACE ( 'NONE', ( #1712 ), #2893, .T. ) ;
#2553 = CARTESIAN_POINT ( 'NONE',  ( 35.50982285435565444, -0.1975270956567271863, 16.49834805537326687 ) ) ;
#2554 = CARTESIAN_POINT ( 'NONE',  ( 37.36894289917042045, 0.2103554180567231702, 12.49608260802403237 ) ) ;
#2555 = ORIENTED_EDGE ( 'NONE', *, *, #1701, .T. ) ;
#2556 = EDGE_CURVE ( 'NONE', #1342, #2807, #1219, .T. ) ;
#2557 = DIRECTION ( 'NONE',  ( 0.000000000000000000, 0.000000000000000000, -1.000000000000000000 ) ) ;
#2558 = ADVANCED_FACE ( 'NONE', ( #164 ), #2399, .F. ) ;
#2559 = AXIS2_PLACEMENT_3D ( 'NONE', #655, #375, #408 ) ;
#2560 = DIRECTION ( 'NONE',  ( -2.312964634635742957E-16, 1.000000000000000000, -0.000000000000000000 ) ) ;
#2561 = ORIENTED_EDGE ( 'NONE', *, *, #713, .F. ) ;
#2562 = VECTOR ( 'NONE', #1791, 1000.000000000000227 ) ;
#2563 = LINE ( 'NONE', #1154, #1112 ) ;
#2564 = AXIS2_PLACEMENT_3D ( 'NONE', #2291, #1028, #1275 ) ;
#2565 = VECTOR ( 'NONE', #1035, 1000.000000000000000 ) ;
#2566 = APPLICATION_CONTEXT ( 'automotive_design' ) ;
#2567 = ORIENTED_EDGE ( 'NONE', *, *, #3166, .T. ) ;
#2568 = ORIENTED_EDGE ( 'NONE', *, *, #1619, .T. ) ;
#2569 = LINE ( 'NONE', #350, #1801 ) ;
#2570 = DIRECTION ( 'NONE',  ( 0.000000000000000000, 0.000000000000000000, 1.000000000000000000 ) ) ;
#2571 = EDGE_CURVE ( 'NONE', #1621, #2847, #2678, .T. ) ;
#2572 = ORIENTED_EDGE ( 'NONE', *, *, #2343, .T. ) ;
#2573 = DIRECTION ( 'NONE',  ( -0.000000000000000000, 0.5000000000000003331, -0.8660254037844383745 ) ) ;
#2574 = DIRECTION ( 'NONE',  ( -0.000000000000000000, -0.5000000000000003331, -0.8660254037844383745 ) ) ;
#2575 = ADVANCED_FACE ( 'NONE', ( #1209 ), #2953, .T. ) ;
#2576 = ORIENTED_EDGE ( 'NONE', *, *, #1753, .T. ) ;
#2577 = EDGE_LOOP ( 'NONE', ( #2601, #305, #2462, #2872, #763 ) ) ;
#2578 = FACE_OUTER_BOUND ( 'NONE', #507, .T. ) ;
#2579 = VECTOR ( 'NONE', #1668, 1000.000000000000000 ) ;
#2580 = AXIS2_PLACEMENT_3D ( 'NONE', #2494, #2987, #1806 ) ;
#2581 = CARTESIAN_POINT ( 'NONE',  ( 60.00000000000000000, -6.928842772166554697E-15, 7.500000000000000000 ) ) ;
#2582 = EDGE_LOOP ( 'NONE', ( #1319, #1637, #617, #2939 ) ) ;
#2583 = LINE ( 'NONE', #593, #392 ) ;
#2584 = CARTESIAN_POINT ( 'NONE',  ( 36.89467617017582768, 0.3922992574225385165, 12.48458637193150089 ) ) ;
#2585 = ORIENTED_EDGE ( 'NONE', *, *, #731, .F. ) ;
#2586 = DIRECTION ( 'NONE',  ( 1.000000000000000000, 2.312964634635742957E-16, 0.000000000000000000 ) ) ;
#2587 = DIRECTION ( 'NONE',  ( 1.000000000000000000, 2.312964634635742957E-16, 0.000000000000000000 ) ) ;
#2588 =( LENGTH_UNIT ( ) NAMED_UNIT ( * ) SI_UNIT ( .MILLI., .METRE. ) );
#2589 = ORIENTED_EDGE ( 'NONE', *, *, #2062, .F. ) ;
#2590 = ORIENTED_EDGE ( 'NONE', *, *, #3208, .T. ) ;
#2591 = SHAPE_REPRESENTATION ( 'Ratchet Stop Thimble Cap', ( #2878 ), #1375 ) ;
#2592 = FACE_OUTER_BOUND ( 'NONE', #2582, .T. ) ;
#2593 = EDGE_CURVE ( 'NONE', #1178, #2825, #1197, .T. ) ;
#2594 = FACE_OUTER_BOUND ( 'NONE', #2133, .T. ) ;
#2595 = EDGE_CURVE ( 'NONE', #2769, #1084, #467, .T. ) ;
#2596 = AXIS2_PLACEMENT_3D ( 'NONE', #782, #1534, #118 ) ;
#2597 = FACE_OUTER_BOUND ( 'NONE', #921, .T. ) ;
#2598 = ORIENTED_EDGE ( 'NONE', *, *, #510, .F. ) ;
#2599 = CARTESIAN_POINT ( 'NONE',  ( 1.649999999999999911, 0.000000000000000000, 0.000000000000000000 ) ) ;
#2600 = AXIS2_PLACEMENT_3D ( 'NONE', #1469, #1726, #727 ) ;
#2601 = ORIENTED_EDGE ( 'NONE', *, *, #1912, .T. ) ;
#2602 = DIRECTION ( 'NONE',  ( 1.000000000000000000, 0.000000000000000000, 0.000000000000000000 ) ) ;
#2603 = EDGE_LOOP ( 'NONE', ( #1929, #2905, #3039 ) ) ;
#2604 = CARTESIAN_POINT ( 'NONE',  ( 1.040000000000000036, -1.154700538379251684, -1.199226976249124676E-17 ) ) ;
#2605 = CARTESIAN_POINT ( 'NONE',  ( 37.00000000000000000, 1.474514954580286030E-14, 13.99999999999999822 ) ) ;
#2606 = CARTESIAN_POINT ( 'NONE',  ( 0.000000000000000000, 0.000000000000000000, 0.000000000000000000 ) ) ;
#2607 = ORIENTED_EDGE ( 'NONE', *, *, #598, .F. ) ;
#2608 = ORIENTED_EDGE ( 'NONE', *, *, #2997, .F. ) ;
#2609 = CARTESIAN_POINT ( 'NONE',  ( 60.00000000000000000, -5.826660652933936785E-15, -1.499999999999999556 ) ) ;
#2610 = CIRCLE ( 'NONE', #110, 1.499999999999999556 ) ;
#2611 = DIRECTION ( 'NONE',  ( 0.000000000000000000, 0.000000000000000000, -1.000000000000000000 ) ) ;
#2612 = MECHANICAL_DESIGN_GEOMETRIC_PRESENTATION_REPRESENTATION (  '', ( #595 ), #1582 ) ;
#2613 = EDGE_CURVE ( 'NONE', #2394, #479, #2712, .T. ) ;
#2614 = VECTOR ( 'NONE', #1347, 1000.000000000000000 ) ;
#2615 = AXIS2_PLACEMENT_3D ( 'NONE', #996, #1559, #2034 ) ;
#2616 = VECTOR ( 'NONE', #2304, 1000.000000000000000 ) ;
#2617 = PRODUCT ( 'Rotary Thimble Outer Sleeve', 'Rotary Thimble Outer Sleeve', '', ( #168 ) ) ;
#2618 = CARTESIAN_POINT ( 'NONE',  ( 47.00000000000000000, 1.133017633246824530E-14, 7.500000000000000000 ) ) ;
#2619 = EDGE_CURVE ( 'NONE', #2676, #401, #1949, .T. ) ;
#2620 = ORIENTED_EDGE ( 'NONE', *, *, #2828, .F. ) ;
#2621 = DIRECTION ( 'NONE',  ( -0.000000000000000000, -0.000000000000000000, 1.000000000000000000 ) ) ;
#2622 =( GEOMETRIC_REPRESENTATION_CONTEXT ( 3 ) GLOBAL_UNCERTAINTY_ASSIGNED_CONTEXT ( ( #444 ) ) GLOBAL_UNIT_ASSIGNED_CONTEXT ( ( #3138, #2664, #441 ) ) REPRESENTATION_CONTEXT ( 'NONE', 'WORKASPACE' ) );
#2623 =( GEOMETRIC_REPRESENTATION_CONTEXT ( 3 ) GLOBAL_UNCERTAINTY_ASSIGNED_CONTEXT ( ( #2423 ) ) GLOBAL_UNIT_ASSIGNED_CONTEXT ( ( #1413, #925, #2991 ) ) REPRESENTATION_CONTEXT ( 'NONE', 'WORKASPACE' ) );
#2624 = VERTEX_POINT ( 'NONE', #2448 ) ;
#2625 = DIRECTION ( 'NONE',  ( 1.000000000000000000, 0.000000000000000000, 0.000000000000000000 ) ) ;
#2626 = ORIENTED_EDGE ( 'NONE', *, *, #3019, .F. ) ;
#2627 = CARTESIAN_POINT ( 'NONE',  ( 140.0000000000000000, -6.928842772166554697E-15, 7.500000000000000000 ) ) ;
#2628 = ADVANCED_FACE ( 'NONE', ( #2386 ), #148, .T. ) ;
#2629 = CARTESIAN_POINT ( 'NONE',  ( 47.00000000000000000, 1.133017633246824530E-14, -1.499999999999994449 ) ) ;
#2630 = CARTESIAN_POINT ( 'NONE',  ( 0.000000000000000000, 0.000000000000000000, 0.000000000000000000 ) ) ;
#2631 = ORIENTED_EDGE ( 'NONE', *, *, #51, .F. ) ;
#2632 = FACE_OUTER_BOUND ( 'NONE', #88, .T. ) ;
#2633 = EDGE_CURVE ( 'NONE', #2118, #310, #1990, .T. ) ;
#2634 = CYLINDRICAL_SURFACE ( 'NONE', #590, 12.00000000000000000 ) ;
#2635 = DIRECTION ( 'NONE',  ( -0.000000000000000000, 1.000000000000000000, -0.000000000000000000 ) ) ;
#2636 = VERTEX_POINT ( 'NONE', #1679 ) ;
#2637 = VECTOR ( 'NONE', #919, 1000.000000000000000 ) ;
#2638 = CARTESIAN_POINT ( 'NONE',  ( 1.649999999999999911, 0.000000000000000000, 1.599999999999999645 ) ) ;
#2639 = EDGE_CURVE ( 'NONE', #466, #3130, #1571, .T. ) ;
#2640 = ORIENTED_EDGE ( 'NONE', *, *, #1483, .F. ) ;
#2641 = CARTESIAN_POINT ( 'NONE',  ( 1.040000000000000036, 0.5773502691896263972, -1.000000000000000000 ) ) ;
#2642 = ORIENTED_EDGE ( 'NONE', *, *, #7, .F. ) ;
#2643 = DIRECTION ( 'NONE',  ( 0.000000000000000000, 0.000000000000000000, -1.000000000000000000 ) ) ;
#2644 = CARTESIAN_POINT ( 'NONE',  ( 100.0000000000000000, -6.316519372592878167E-15, 2.499999999999999556 ) ) ;
#2645 = CARTESIAN_POINT ( 'NONE',  ( 0.000000000000000000, 0.000000000000000000, 0.000000000000000000 ) ) ;
#2646 = ORIENTED_EDGE ( 'NONE', *, *, #733, .F. ) ;
#2647 = DIRECTION ( 'NONE',  ( 0.000000000000000000, 0.000000000000000000, -1.000000000000000000 ) ) ;
#2648 = FILL_AREA_STYLE ('',( #2421 ) ) ;
#2649 = DIRECTION ( 'NONE',  ( -1.000000000000000000, -0.000000000000000000, -0.000000000000000000 ) ) ;
#2650 = ORIENTED_EDGE ( 'NONE', *, *, #2497, .F. ) ;
#2651 = AXIS2_PLACEMENT_3D ( 'NONE', #1236, #750, #511 ) ;
#2652 = CARTESIAN_POINT ( 'NONE',  ( 36.80088933932603368, 1.499879510127410498, 16.37414004115125721 ) ) ;
#2653 = ORIENTED_EDGE ( 'NONE', *, *, #1189, .T. ) ;
#2654 = DIRECTION ( 'NONE',  ( -1.000000000000000000, -0.000000000000000000, -0.000000000000000000 ) ) ;
#2655 = ORIENTED_EDGE ( 'NONE', *, *, #3019, .T. ) ;
#2656 = EDGE_CURVE ( 'NONE', #357, #1678, #2089, .T. ) ;
#2657 = CARTESIAN_POINT ( 'NONE',  ( 180.0000000000000284, -6.928842772166554697E-15, 7.500000000000000000 ) ) ;
#2658 = UNCERTAINTY_MEASURE_WITH_UNIT (LENGTH_MEASURE( 1.000000000000000082E-05 ), #1959, 'distance_accuracy_value', 'NONE');
#2659 = LINE ( 'NONE', #715, #1888 ) ;
#2660 = DIRECTION ( 'NONE',  ( 0.000000000000000000, 1.000000000000000000, 0.000000000000000000 ) ) ;
#2661 = SHAPE_DEFINITION_REPRESENTATION ( #1109, #330 ) ;
#2662 = ADVANCED_FACE ( 'NONE', ( #480 ), #2463, .T. ) ;
#2663 = CARTESIAN_POINT ( 'NONE',  ( 41.99999999999999289, -15.00000000000000355, 0.000000000000000000 ) ) ;
#2664 =( NAMED_UNIT ( * ) PLANE_ANGLE_UNIT ( ) SI_UNIT ( $, .RADIAN. ) );
#2665 = AXIS2_PLACEMENT_3D ( 'NONE', #2171, #719, #2419 ) ;
#2666 = AXIS2_PLACEMENT_3D ( 'NONE', #3086, #1380, #1137 ) ;
#2667 = DIRECTION ( 'NONE',  ( 1.000000000000000000, -0.000000000000000000, -0.000000000000000000 ) ) ;
#2668 = VECTOR ( 'NONE', #582, 1000.000000000000000 ) ;
#2669 = PLANE ( 'NONE',  #1602 ) ;
#2670 = VECTOR ( 'NONE', #1913, 1000.000000000000000 ) ;
#2671 = VECTOR ( 'NONE', #2941, 1000.000000000000000 ) ;
#2672 = ORIENTED_EDGE ( 'NONE', *, *, #1686, .T. ) ;
#2673 = CARTESIAN_POINT ( 'NONE',  ( 30.00000000000000355, -13.99999999999999467, 7.500000000000001776 ) ) ;
#2674 = AXIS2_PLACEMENT_3D ( 'NONE', #145, #1418, #1945 ) ;
#2675 = CIRCLE ( 'NONE', #1271, 7.500000000000000000 ) ;
#2676 = VERTEX_POINT ( 'NONE', #453 ) ;
#2677 = STYLED_ITEM ( 'NONE', ( #343 ), #824 ) ;
#2678 = LINE ( 'NONE', #1390, #535 ) ;
#2679 = EDGE_CURVE ( 'NONE', #241, #2624, #1425, .T. ) ;
#2680 = PLANE ( 'NONE',  #102 ) ;
#2681 =( REPRESENTATION_RELATIONSHIP ('NONE','NONE', #2426, #514 ) REPRESENTATION_RELATIONSHIP_WITH_TRANSFORMATION ( #995 )SHAPE_REPRESENTATION_RELATIONSHIP( ) );
#2682 = CARTESIAN_POINT ( 'NONE',  ( 7.650000000000000355, 0.000000000000000000, 0.000000000000000000 ) ) ;
#2683 = APPLICATION_PROTOCOL_DEFINITION ( 'draft international standard', 'automotive_design', 1998, #2566 ) ;
#2684 = ADVANCED_FACE ( 'NONE', ( #729 ), #2708, .F. ) ;
#2685 = CARTESIAN_POINT ( 'NONE',  ( 60.00000000000000000, -6.928842772166554697E-15, 7.500000000000000000 ) ) ;
#2686 = APPLICATION_PROTOCOL_DEFINITION ( 'draft international standard', 'automotive_design', 1998, #642 ) ;
#2687 = FACE_OUTER_BOUND ( 'NONE', #841, .T. ) ;
#2688 = DIRECTION ( 'NONE',  ( 1.000000000000000000, 0.000000000000000000, 0.000000000000000000 ) ) ;
#2689 = VERTEX_POINT ( 'NONE', #186 ) ;
#2690 = SURFACE_STYLE_USAGE ( .BOTH. , #2194 ) ;
#2691 = VECTOR ( 'NONE', #835, 1000.000000000000000 ) ;
#2692 = ORIENTED_EDGE ( 'NONE', *, *, #3060, .F. ) ;
#2693 = DIRECTION ( 'NONE',  ( -0.000000000000000000, -1.000000000000000000, -0.000000000000000000 ) ) ;
#2694 = AXIS2_PLACEMENT_3D ( 'NONE', #3144, #2409, #179 ) ;
#2695 = CARTESIAN_POINT ( 'NONE',  ( 38.19275052663392245, -0.9148478194932491148, 16.45375607287288133 ) ) ;
#2696 = LINE ( 'NONE', #2467, #2501 ) ;
#2697 = DIRECTION ( 'NONE',  ( -1.000000000000000000, -0.000000000000000000, -0.000000000000000000 ) ) ;
#2698 = CONTEXT_DEPENDENT_SHAPE_REPRESENTATION ( #2681, #2883 ) ;
#2699 =( NAMED_UNIT ( * ) SI_UNIT ( $, .STERADIAN. ) SOLID_ANGLE_UNIT ( ) );
#2700 = DIRECTION ( 'NONE',  ( 1.000000000000000000, -0.000000000000000000, -0.000000000000000000 ) ) ;
#2701 = EDGE_CURVE ( 'NONE', #1030, #1076, #1094, .T. ) ;
#2702 = DIRECTION ( 'NONE',  ( -1.000000000000000000, -0.000000000000000000, -0.000000000000000000 ) ) ;
#2703 = DIRECTION ( 'NONE',  ( -1.000000000000000000, -0.000000000000000000, -0.000000000000000000 ) ) ;
#2704 = ORIENTED_EDGE ( 'NONE', *, *, #270, .T. ) ;
#2705 = ORIENTED_EDGE ( 'NONE', *, *, #931, .T. ) ;
#2706 = CARTESIAN_POINT ( 'NONE',  ( 1.040000000000000036, -0.5773502691896253980, -1.000000000000000000 ) ) ;
#2707 = CARTESIAN_POINT ( 'NONE',  ( 37.92226537325434776, -1.198992358192654484, 16.42086068928975706 ) ) ;
#2708 = PLANE ( 'NONE',  #790 ) ;
#2709 = FACE_OUTER_BOUND ( 'NONE', #1932, .T. ) ;
#2710 = B_SPLINE_CURVE_WITH_KNOTS ( 'NONE', 3,
 ( #327, #2751, #2022, #3061, #2783, #1781, #71, #1549, #1248, #526, #2038, #1314, #2798, #2534, #1071, #2055, #1532, #2283, #2523, #1002, #825, #1824, #1798, #3026, #796, #508, #54, #561 ),
 .UNSPECIFIED., .F., .F.,
 ( 4, 2, 2, 2, 2, 2, 2, 2, 2, 2, 2, 2, 2, 4 ),
 ( 0.000000000000000000, 0.0002936178373947212505, 0.0005872356747894425010, 0.0008808535121841636973, 0.001174471349578885002, 0.001761707024368327828, 0.002348942699157770871, 0.002642560536552492501, 0.002936178373947213264, 0.003523414048736636574, 0.003817031886131348663, 0.004110649723526061186, 0.004404267560920773275, 0.004697885398315485364 ),
 .UNSPECIFIED. ) ;
#2711 = PLANE ( 'NONE',  #1998 ) ;
#2712 = CIRCLE ( 'NONE', #2150, 5.000000000000000000 ) ;
#2713 = VERTEX_POINT ( 'NONE', #682 ) ;
#2714 = EDGE_CURVE ( 'NONE', #2974, #1415, #2659, .T. ) ;
#2715 = DIRECTION ( 'NONE',  ( 1.000000000000000000, 0.000000000000000000, 0.000000000000000000 ) ) ;
#2716 = PRODUCT ( 'frame', 'frame', '', ( #485 ) ) ;
#2717 = DIRECTION ( 'NONE',  ( -0.000000000000000000, 0.000000000000000000, -1.000000000000000000 ) ) ;
#2718 = CIRCLE ( 'NONE', #1792, 7.500000000000000000 ) ;
#2719 = ORIENTED_EDGE ( 'NONE', *, *, #104, .F. ) ;
#2720 = EDGE_CURVE ( 'NONE', #916, #3031, #1229, .T. ) ;
#2721 = VERTEX_POINT ( 'NONE', #1728 ) ;
#2722 = CIRCLE ( 'NONE', #2312, 5.000000000000000888 ) ;
#2723=STYLED_ITEM('',(#3257),#3192);
#2724 = AXIS2_PLACEMENT_3D ( 'NONE', #385, #2808, #1833 ) ;
#2725 = CIRCLE ( 'NONE', #850, 1.250000000000001110 ) ;
#2726 = DIRECTION ( 'NONE',  ( 0.000000000000000000, 1.000000000000000000, 0.000000000000000000 ) ) ;
#2727 = DIRECTION ( 'NONE',  ( 0.000000000000000000, 0.8660254037844384856, 0.5000000000000004441 ) ) ;
#2728 = FACE_OUTER_BOUND ( 'NONE', #2119, .T. ) ;
#2729 = ITEM_DEFINED_TRANSFORMATION ( 'NONE', 'NONE', #754,  #2878 ) ;
#2730 = ADVANCED_FACE ( 'NONE', ( #741 ), #3150, .F. ) ;
#2731 = CARTESIAN_POINT ( 'NONE',  ( 140.0000000000000000, -6.928842772166554697E-15, 7.500000000000000000 ) ) ;
#2732 = ADVANCED_FACE ( 'NONE', ( #483 ), #3072, .T. ) ;
#2733 = COLOUR_RGB ( '',0.8941176470588234615, 0.8941176470588234615, 0.8941176470588234615 ) ;
#2734 = CARTESIAN_POINT ( 'NONE',  ( 87.00000000000000000, -7.622732162557277534E-15, 7.500000000000000000 ) ) ;
#2735 = ORIENTED_EDGE ( 'NONE', *, *, #2326, .T. ) ;
#2736 = ADVANCED_FACE ( 'NONE', ( #1967 ), #3185, .F. ) ;
#2737 = LINE ( 'NONE', #2253, #2162 ) ;
#2738 = CARTESIAN_POINT ( 'NONE',  ( 7.650000000000000355, 0.000000000000000000, 0.000000000000000000 ) ) ;
#2739 = VERTEX_POINT ( 'NONE', #1922 ) ;
#2740 = ORIENTED_EDGE ( 'NONE', *, *, #882, .T. ) ;
#2741 = APPLICATION_CONTEXT ( 'automotive_design' ) ;
#2742 = EDGE_CURVE ( 'NONE', #2807, #1342, #2454, .T. ) ;
#2743 = CYLINDRICAL_SURFACE ( 'NONE', #1536, 9.000000000000001776 ) ;
#2744 = AXIS2_PLACEMENT_3D ( 'NONE', #1133, #2131, #3113 ) ;
#2745 = DIRECTION ( 'NONE',  ( 1.000000000000000000, 2.312964634635742957E-16, -0.000000000000000000 ) ) ;
#2746 = CARTESIAN_POINT ( 'NONE',  ( 36.58213974117526845, -0.1061009270805697569, 12.50000000000000000 ) ) ;
#2747 = FACE_OUTER_BOUND ( 'NONE', #1986, .T. ) ;
#2748 = AXIS2_PLACEMENT_3D ( 'NONE', #413, #641, #1366 ) ;
#2749 = FACE_OUTER_BOUND ( 'NONE', #2781, .T. ) ;
#2750 = ORIENTED_EDGE ( 'NONE', *, *, #1192, .T. ) ;
#2751 = CARTESIAN_POINT ( 'NONE',  ( 38.49999999999999289, 0.09929498707318666628, 16.49999999999999289 ) ) ;
#2752 = CARTESIAN_POINT ( 'NONE',  ( 37.00000000000000000, 1.474514954580286030E-14, 20.99999999999999645 ) ) ;
#2753 = DIRECTION ( 'NONE',  ( -1.000000000000000000, -0.000000000000000000, -0.000000000000000000 ) ) ;
#2754 = EDGE_LOOP ( 'NONE', ( #2413, #2156, #2719, #944 ) ) ;
#2755 = ORIENTED_EDGE ( 'NONE', *, *, #2084, .T. ) ;
#2756 = CARTESIAN_POINT ( 'NONE',  ( 100.0000000000000000, -6.928842772166554697E-15, 7.500000000000000000 ) ) ;
#2757 = CARTESIAN_POINT ( 'NONE',  ( 37.91396272957889124, -1.193436492094909429, 16.42069107455876775 ) ) ;
#2758 = CARTESIAN_POINT ( 'NONE',  ( 37.00000000000000000, 1.474514954580286030E-14, 12.99999999999999822 ) ) ;
#2759 = EDGE_CURVE ( 'NONE', #2739, #1365, #1685, .T. ) ;
#2760 = FACE_OUTER_BOUND ( 'NONE', #449, .T. ) ;
#2761 = EDGE_CURVE ( 'NONE', #2825, #1860, #2696, .T. ) ;
#2762 = PRODUCT_DEFINITION_CONTEXT ( 'detailed design', #1850, 'design' ) ;
#2763 = SURFACE_STYLE_USAGE ( .BOTH. , #2052 ) ;
#2764 =( NAMED_UNIT ( * ) PLANE_ANGLE_UNIT ( ) SI_UNIT ( $, .RADIAN. ) );
#2765 = ORIENTED_EDGE ( 'NONE', *, *, #465, .F. ) ;
#2766 = CARTESIAN_POINT ( 'NONE',  ( 1.040000000000000036, -0.5773502691896253980, 1.000000000000000000 ) ) ;
#2767 = CARTESIAN_POINT ( 'NONE',  ( 38.49999999999999289, 1.474514954580286030E-14, 20.99999999999999645 ) ) ;
#2768 = SURFACE_SIDE_STYLE ('',( #1815 ) ) ;
#2769 = VERTEX_POINT ( 'NONE', #236 ) ;
#2770 = AXIS2_PLACEMENT_3D ( 'NONE', #1360, #120, #1631 ) ;
#2771 = PRODUCT ( 'Ratchet Stop Thimble Cap', 'Ratchet Stop Thimble Cap', '', ( #903 ) ) ;
#2772 = DIRECTION ( 'NONE',  ( 0.000000000000000000, 0.000000000000000000, -1.000000000000000000 ) ) ;
#2773 = CARTESIAN_POINT ( 'NONE',  ( 35.50000000000000000, -0.1959257125632785645, 16.49999999999999289 ) ) ;
#2774 = DIRECTION ( 'NONE',  ( 1.000000000000000000, 0.000000000000000000, 0.000000000000000000 ) ) ;
#2775 = AXIS2_PLACEMENT_3D ( 'NONE', #1657, #124, #2122 ) ;
#2776 = VERTEX_POINT ( 'NONE', #2228 ) ;
#2777 = DIRECTION ( 'NONE',  ( -3.854941057726240069E-16, 1.000000000000000000, 0.000000000000000000 ) ) ;
#2778 = AXIS2_PLACEMENT_3D ( 'NONE', #666, #1965, #1935 ) ;
#2779 = EDGE_CURVE ( 'NONE', #815, #2850, #1519, .T. ) ;
#2780 = CARTESIAN_POINT ( 'NONE',  ( -41.99999999999999289, -6.449497959004950529E-15, 15.00000000000000000 ) ) ;
#2781 = EDGE_LOOP ( 'NONE', ( #2087, #2208 ) ) ;
#2782 = EDGE_CURVE ( 'NONE', #2965, #974, #2926, .T. ) ;
#2783 = CARTESIAN_POINT ( 'NONE',  ( 38.42308964188128328, 0.4842307372812582611, 16.48742442505516692 ) ) ;
#2784 = CARTESIAN_POINT ( 'NONE',  ( 87.00000000000000000, -7.622732162557277534E-15, 16.49999999999999289 ) ) ;
#2785 = CARTESIAN_POINT ( 'NONE',  ( 37.00000000000000000, 1.474514954580286030E-14, 20.99999999999999645 ) ) ;
#2786 = EDGE_LOOP ( 'NONE', ( #830, #2341, #1043, #2646, #2999 ) ) ;
#2787 = EDGE_LOOP ( 'NONE', ( #2097, #962, #1785, #3013, #1567, #2908, #1538, #2631 ) ) ;
#2788 = DIRECTION ( 'NONE',  ( -1.000000000000000000, -0.000000000000000000, -0.000000000000000000 ) ) ;
#2789 = CARTESIAN_POINT ( 'NONE',  ( 1.040000000000000036, -0.5773502691896253980, 1.000000000000000000 ) ) ;
#2790 = CARTESIAN_POINT ( 'NONE',  ( 87.00000000000000000, -7.622732162557277534E-15, 12.50000000000000000 ) ) ;
#2791 = ORIENTED_EDGE ( 'NONE', *, *, #497, .F. ) ;
#2792 = DIRECTION ( 'NONE',  ( 1.000000000000000000, 0.000000000000000000, -0.000000000000000000 ) ) ;
#2793 = DIRECTION ( 'NONE',  ( -1.000000000000000000, -0.000000000000000000, -0.000000000000000000 ) ) ;
#2794 =( LENGTH_UNIT ( ) NAMED_UNIT ( * ) SI_UNIT ( .MILLI., .METRE. ) );
#2795 = EDGE_LOOP ( 'NONE', ( #946, #523, #2537, #2840 ) ) ;
#2796 = AXIS2_PLACEMENT_3D ( 'NONE', #187, #936, #1185 ) ;
#2797 = ADVANCED_FACE ( 'NONE', ( #1699, #1471 ), #2680, .F. ) ;
#2798 = CARTESIAN_POINT ( 'NONE',  ( 37.19662223785018540, 1.499925442620323235, 16.37413227714582220 ) ) ;
#2799 = DIRECTION ( 'NONE',  ( 0.000000000000000000, 0.000000000000000000, 1.000000000000000000 ) ) ;
#2800 = EDGE_CURVE ( 'NONE', #914, #3197, #950, .T. ) ;
#2801 = APPLICATION_CONTEXT ( 'automotive_design' ) ;
#2802 = ADVANCED_FACE ( 'NONE', ( #2275 ), #1014, .T. ) ;
#2803 = EDGE_LOOP ( 'NONE', ( #2307, #2817 ) ) ;
#2804 = ORIENTED_EDGE ( 'NONE', *, *, #3093, .F. ) ;
#2805 = CARTESIAN_POINT ( 'NONE',  ( 35.54829862735516599, -0.3901384415568707742, 16.49205630963118807 ) ) ;
#2806 = CARTESIAN_POINT ( 'NONE',  ( 35.53942839536624376, -0.3936020622859607854, 16.49320894598177034 ) ) ;
#2807 = VERTEX_POINT ( 'NONE', #1492 ) ;
#2808 = DIRECTION ( 'NONE',  ( -1.000000000000000000, -0.000000000000000000, -0.000000000000000000 ) ) ;
#2809 = LINE ( 'NONE', #648, #460 ) ;
#2810 = SURFACE_SIDE_STYLE ('',( #822 ) ) ;
#2811 = PRESENTATION_LAYER_ASSIGNMENT (  '', '', ( #881 ) ) ;
#2812 = EDGE_LOOP ( 'NONE', ( #2251, #1056, #2128, #2750 ) ) ;
#2813 = AXIS2_PLACEMENT_3D ( 'NONE', #3205, #2928, #968 ) ;
#2814 = DIRECTION ( 'NONE',  ( -1.000000000000000000, -0.000000000000000000, -0.000000000000000000 ) ) ;
#2815 = SHAPE_REPRESENTATION_RELATIONSHIP ( 'NONE' , 'NONE' ,  #514, #1050 ) ;
#2816 = ADVANCED_FACE ( 'NONE', ( #2064 ), #1204, .F. ) ;
#2817 = ORIENTED_EDGE ( 'NONE', *, *, #2084, .F. ) ;
#2818 = VERTEX_POINT ( 'NONE', #1556 ) ;
#2819 = CARTESIAN_POINT ( 'NONE',  ( 35.50000000000000000, -7.622732095468789599E-15, 16.49999999999999289 ) ) ;
#2820 = CARTESIAN_POINT ( 'NONE',  ( 155.0000000000000284, -6.928842772166554697E-15, 7.500000000000000000 ) ) ;
#2821 = VERTEX_POINT ( 'NONE', #33 ) ;
#2822 = DIRECTION ( 'NONE',  ( 0.000000000000000000, -1.000000000000000000, 0.000000000000000000 ) ) ;
#2823 = DIRECTION ( 'NONE',  ( 1.000000000000000000, 2.312964634635742957E-16, 0.000000000000000000 ) ) ;
#2824 = SURFACE_STYLE_USAGE ( .BOTH. , #1527 ) ;
#2825 = VERTEX_POINT ( 'NONE', #3034 ) ;
#2826 = DIRECTION ( 'NONE',  ( 1.000000000000000000, 0.000000000000000000, 0.000000000000000000 ) ) ;
#2827 = COLOUR_RGB ( '',0.8941176470588234615, 0.8941176470588234615, 0.8941176470588234615 ) ;
#2828 = EDGE_CURVE ( 'NONE', #3117, #2092, #1627, .T. ) ;
#2829 = DIRECTION ( 'NONE',  ( 0.000000000000000000, 0.000000000000000000, -1.000000000000000000 ) ) ;
#2830 = EDGE_LOOP ( 'NONE', ( #2561, #2126 ) ) ;
#2831 = PRODUCT_DEFINITION_FORMATION_WITH_SPECIFIED_SOURCE ( 'ANY', '', #1647, .NOT_KNOWN. ) ;
#2832 = CARTESIAN_POINT ( 'NONE',  ( 36.61043004145795265, -1.451850406891351364, 16.38214551140935882 ) ) ;
#2833 = CARTESIAN_POINT ( 'NONE',  ( 87.00000000000000000, -7.622732162557277534E-15, 16.49999999999999289 ) ) ;
#2834 = ORIENTED_EDGE ( 'NONE', *, *, #456, .F. ) ;
#2835 = ADVANCED_FACE ( 'NONE', ( #302 ), #3016, .T. ) ;
#2836 = DIRECTION ( 'NONE',  ( 0.000000000000000000, 1.000000000000000000, 0.000000000000000000 ) ) ;
#2837 = CARTESIAN_POINT ( 'NONE',  ( 1.649999999999999911, 0.000000000000000000, 2.849999999999999645 ) ) ;
#2838 = DIRECTION ( 'NONE',  ( 0.000000000000000000, 0.000000000000000000, 1.000000000000000000 ) ) ;
#2839 = VERTEX_POINT ( 'NONE', #1063 ) ;
#2840 = ORIENTED_EDGE ( 'NONE', *, *, #101, .T. ) ;
#2841 = CYLINDRICAL_SURFACE ( 'NONE', #1780, 1.499999999999999556 ) ;
#2842 = DIRECTION ( 'NONE',  ( -1.000000000000000000, -0.000000000000000000, -0.000000000000000000 ) ) ;
#2843 =( NAMED_UNIT ( * ) SI_UNIT ( $, .STERADIAN. ) SOLID_ANGLE_UNIT ( ) );
#2844 = VECTOR ( 'NONE', #2793, 1000.000000000000000 ) ;
#2845 = AXIS2_PLACEMENT_3D ( 'NONE', #1126, #400, #2142 ) ;
#2846 = LINE ( 'NONE', #3124, #1695 ) ;
#2847 = VERTEX_POINT ( 'NONE', #805 ) ;
#2848 = ORIENTED_EDGE ( 'NONE', *, *, #354, .F. ) ;
#2849 = CARTESIAN_POINT ( 'NONE',  ( 140.0000000000000000, -6.928842772166554697E-15, 7.500000000000000000 ) ) ;
#2850 = VERTEX_POINT ( 'NONE', #1305 ) ;
#2851 = DIRECTION ( 'NONE',  ( 1.000000000000000000, 2.312964634635742957E-16, -0.000000000000000000 ) ) ;
#2852 = EDGE_CURVE ( 'NONE', #1890, #3213, #1240, .T. ) ;
#2853 = LINE ( 'NONE', #82, #3104 ) ;
#2854 = PRODUCT_DEFINITION ( 'UNKNOWN', '', #1540, #1190 ) ;
#2855 = ORIENTED_EDGE ( 'NONE', *, *, #2714, .F. ) ;
#2856 = EDGE_LOOP ( 'NONE', ( #2863, #2339, #1225, #2060, #299, #2642 ) ) ;
#2857 = DIRECTION ( 'NONE',  ( 1.000000000000000000, 0.000000000000000000, 0.000000000000000000 ) ) ;
#2858 = FACE_BOUND ( 'NONE', #1096, .T. ) ;
#2859 = COLOUR_RGB ( '',0.8941176470588234615, 0.8941176470588234615, 0.8941176470588234615 ) ;
#2860 = UNCERTAINTY_MEASURE_WITH_UNIT (LENGTH_MEASURE( 1.000000000000000082E-05 ), #2794, 'distance_accuracy_value', 'NONE');
#2861 =( REPRESENTATION_RELATIONSHIP ('NONE','NONE', #2426, #2591 ) REPRESENTATION_RELATIONSHIP_WITH_TRANSFORMATION ( #1999 )SHAPE_REPRESENTATION_RELATIONSHIP( ) );
#2862 = DIRECTION ( 'NONE',  ( 1.000000000000000000, 0.000000000000000000, 0.000000000000000000 ) ) ;
#2863 = ORIENTED_EDGE ( 'NONE', *, *, #273, .F. ) ;
#2864 = EDGE_CURVE ( 'NONE', #2348, #2839, #1506, .T. ) ;
#2865 = CARTESIAN_POINT ( 'NONE',  ( 37.19571985532142122, 1.490394421081202125, 16.37575894629744866 ) ) ;
#2866 = ORIENTED_EDGE ( 'NONE', *, *, #1092, .T. ) ;
#2867 = CARTESIAN_POINT ( 'NONE',  ( -41.99999999999999289, -1.109217911451089172E-14, 15.00000000000000000 ) ) ;
#2868 = EDGE_LOOP ( 'NONE', ( #1977, #2301, #2043, #802, #367 ) ) ;
#2869 = FACE_BOUND ( 'NONE', #1855, .T. ) ;
#2870 = DIRECTION ( 'NONE',  ( 0.000000000000000000, 0.000000000000000000, 1.000000000000000000 ) ) ;
#2871 = ORIENTED_EDGE ( 'NONE', *, *, #1329, .T. ) ;
#2872 = ORIENTED_EDGE ( 'NONE', *, *, #151, .F. ) ;
#2873 = CARTESIAN_POINT ( 'NONE',  ( 70.00000000000032685, -6.928842772166554697E-15, 7.500000000000000000 ) ) ;
#2874 = AXIS2_PLACEMENT_3D ( 'NONE', #1972, #2898, #423 ) ;
#2875 = LINE ( 'NONE', #1346, #1213 ) ;
#2876 = SURFACE_STYLE_USAGE ( .BOTH. , #2101 ) ;
#2877 = CLOSED_SHELL ( 'NONE', ( #771, #376, #62, #827 ) ) ;
#2878 = AXIS2_PLACEMENT_3D ( 'NONE', #3071, #2799, #1837 ) ;
#2879 = EDGE_CURVE ( 'NONE', #56, #1709, #818, .T. ) ;
#2880 = TOROIDAL_SURFACE ( 'NONE', #1001, 1.599999999999999645, 0.1000000000000000056 ) ;
#2881 = PRESENTATION_LAYER_ASSIGNMENT (  '', '', ( #2108 ) ) ;
#2882 = VECTOR ( 'NONE', #59, 1000.000000000000000 ) ;
#2883 = PRODUCT_DEFINITION_SHAPE ( 'NONE', 'NONE',  #3223 ) ;
#2884 = FACE_OUTER_BOUND ( 'NONE', #2069, .T. ) ;
#2885 = AXIS2_PLACEMENT_3D ( 'NONE', #1696, #712, #2643 ) ;
#2886 = ORIENTED_EDGE ( 'NONE', *, *, #2477, .F. ) ;
#2887 = CARTESIAN_POINT ( 'NONE',  ( 27.00000000000000355, -13.99999999999999289, 7.500000000000001776 ) ) ;
#2888 = AXIS2_PLACEMENT_3D ( 'NONE', #884, #3115, #616 ) ;
#2889 = ORIENTED_EDGE ( 'NONE', *, *, #2779, .T. ) ;
#2890 = FILL_AREA_STYLE ('',( #1767 ) ) ;
#2891 = ORIENTED_EDGE ( 'NONE', *, *, #1104, .F. ) ;
#2892 = ORIENTED_EDGE ( 'NONE', *, *, #2782, .T. ) ;
#2893 = CYLINDRICAL_SURFACE ( 'NONE', #654, 7.500000000000000000 ) ;
#2894 = DIRECTION ( 'NONE',  ( 2.312964634635742957E-16, -1.000000000000000000, 0.000000000000000000 ) ) ;
#2895 = APPLICATION_PROTOCOL_DEFINITION ( 'draft international standard', 'automotive_design', 1998, #3176 ) ;
#2896 = ORIENTED_EDGE ( 'NONE', *, *, #456, .T. ) ;
#2897 = SURFACE_SIDE_STYLE ('',( #219 ) ) ;
#2898 = DIRECTION ( 'NONE',  ( 1.000000000000000000, 2.312964634635742957E-16, 0.000000000000000000 ) ) ;
#2899 = CIRCLE ( 'NONE', #767, 2.849999999999999645 ) ;
#2900 = ADVANCED_FACE ( 'NONE', ( #1522 ), #2305, .T. ) ;
#2901 = DIRECTION ( 'NONE',  ( 1.000000000000000000, -0.000000000000000000, -0.000000000000000000 ) ) ;
#2902 = ORIENTED_EDGE ( 'NONE', *, *, #566, .T. ) ;
#2903 = AXIS2_PLACEMENT_3D ( 'NONE', #1682, #2217, #2660 ) ;
#2904 = CARTESIAN_POINT ( 'NONE',  ( 4.336808689942017736E-16, 1.424999999999999822, 0.000000000000000000 ) ) ;
#2905 = ORIENTED_EDGE ( 'NONE', *, *, #2536, .T. ) ;
#2906 = EDGE_CURVE ( 'NONE', #1246, #3085, #1702, .T. ) ;
#2907 = DIRECTION ( 'NONE',  ( -1.000000000000000000, 0.000000000000000000, -0.000000000000000000 ) ) ;
#2908 = ORIENTED_EDGE ( 'NONE', *, *, #2720, .F. ) ;
#2909 = DIRECTION ( 'NONE',  ( 1.000000000000000000, 2.312964634635742957E-16, 0.000000000000000000 ) ) ;
#2910 = DIRECTION ( 'NONE',  ( 1.000000000000000000, 2.312964634635742957E-16, 0.000000000000000000 ) ) ;
#2911 = DIRECTION ( 'NONE',  ( -1.000000000000000000, -0.000000000000000000, -0.000000000000000000 ) ) ;
#2912 = DIRECTION ( 'NONE',  ( 1.000000000000000000, 0.000000000000000000, 0.000000000000000000 ) ) ;
#2913 = ORIENTED_EDGE ( 'NONE', *, *, #2556, .F. ) ;
#2914 = SURFACE_STYLE_USAGE ( .BOTH. , #1704 ) ;
#2915 = DIRECTION ( 'NONE',  ( 1.000000000000000000, 0.000000000000000000, 0.000000000000000000 ) ) ;
#2916 = UNCERTAINTY_MEASURE_WITH_UNIT (LENGTH_MEASURE( 1.000000000000000082E-05 ), #3088, 'distance_accuracy_value', 'NONE');
#2917 = LINE ( 'NONE', #940, #1748 ) ;
#2918 = ORIENTED_EDGE ( 'NONE', *, *, #1463, .T. ) ;
#2919 = VECTOR ( 'NONE', #1359, 1000.000000000000000 ) ;
#2920 = CARTESIAN_POINT ( 'NONE',  ( 36.08479696852054275, 1.192462354422088255, 16.42082098627955489 ) ) ;
#2921 = EDGE_CURVE ( 'NONE', #2713, #3117, #1843, .T. ) ;
#2922 = ORIENTED_EDGE ( 'NONE', *, *, #1006, .T. ) ;
#2923 = ORIENTED_EDGE ( 'NONE', *, *, #1606, .F. ) ;
#2924 = EDGE_CURVE ( 'NONE', #1964, #1489, #2273, .T. ) ;
#2925 = LINE ( 'NONE', #693, #2671 ) ;
#2926 = LINE ( 'NONE', #695, #3184 ) ;
#2927 = CARTESIAN_POINT ( 'NONE',  ( -26.99999999999999645, -7.500000000000007105, 7.500000000000000000 ) ) ;
#2928 = DIRECTION ( 'NONE',  ( -1.000000000000000000, -0.000000000000000000, -0.000000000000000000 ) ) ;
#2929 = CARTESIAN_POINT ( 'NONE',  ( 4.336808689942017736E-16, -1.425000000000000044, -2.617682533177466553E-16 ) ) ;
#2930 = CIRCLE ( 'NONE', #1317, 9.000000000000000000 ) ;
#2931 = DIRECTION ( 'NONE',  ( -1.000000000000000000, 0.000000000000000000, 0.000000000000000000 ) ) ;
#2932 = AXIS2_PLACEMENT_3D ( 'NONE', #2482, #570, #2277 ) ;
#2933 = CARTESIAN_POINT ( 'NONE',  ( -30.00000000000000000, -3.673940397442059178E-15, 15.00000000000000000 ) ) ;
#2934 = VECTOR ( 'NONE', #2487, 1000.000000000000000 ) ;
#2935 = VERTEX_POINT ( 'NONE', #3110 ) ;
#2936 = CARTESIAN_POINT ( 'NONE',  ( 0.000000000000000000, 0.000000000000000000, 0.000000000000000000 ) ) ;
#2937 = VECTOR ( 'NONE', #2076, 1000.000000000000000 ) ;
#2938 = AXIS2_PLACEMENT_3D ( 'NONE', #2752, #1005, #2008 ) ;
#2939 = ORIENTED_EDGE ( 'NONE', *, *, #1869, .T. ) ;
#2940 = STYLED_ITEM ( 'NONE', ( #3207 ), #2267 ) ;
#2941 = DIRECTION ( 'NONE',  ( 0.5150380749100542666, 0.000000000000000000, -0.8571673007021122226 ) ) ;
#2942 = CARTESIAN_POINT ( 'NONE',  ( 38.42308964188128328, -0.4842307372812458266, 16.48742442505517047 ) ) ;
#2943 = DIRECTION ( 'NONE',  ( -3.854941057726241055E-16, 1.000000000000000000, 0.000000000000000000 ) ) ;
#2944 = DIRECTION ( 'NONE',  ( -0.000000000000000000, -0.000000000000000000, 1.000000000000000000 ) ) ;
#2945 = EDGE_CURVE ( 'NONE', #2821, #2965, #1747, .T. ) ;
#2946 = B_SPLINE_CURVE_WITH_KNOTS ( 'NONE', 3,
 ( #2274, #949, #3202, #235, #2942, #518, #976, #2695, #468, #2707, #1470, #1228, #2090, #1336, #1073, #2832, #1587, #1062, #1817, #2063, #552, #1027, #365, #1322, #2805, #2553, #1601, #2819 ),
 .UNSPECIFIED., .F., .F.,
 ( 4, 2, 2, 2, 2, 2, 2, 2, 2, 2, 2, 2, 2, 4 ),
 ( 0.000000000000000000, 0.0002936178373947053669, 0.0005872356747894107339, 0.0008808535121841159924, 0.001174471349578821468, 0.001761707024368247597, 0.002348942699157674160, 0.002642560536552387117, 0.002936178373947100507, 0.003523414048736544634, 0.003817031886131267999, 0.004110649723525990930, 0.004404267560920714294, 0.004697885398315436792 ),
 .UNSPECIFIED. ) ;
#2947 = CARTESIAN_POINT ( 'NONE',  ( 1.617350269189632428, 0.000000000000000000, 0.000000000000000000 ) ) ;
#2948 = DIRECTION ( 'NONE',  ( 0.000000000000000000, 0.000000000000000000, -1.000000000000000000 ) ) ;
#2949 = CARTESIAN_POINT ( 'NONE',  ( 87.00000000000000000, -7.622732162557277534E-15, 12.50000000000000000 ) ) ;
#2950 = ORIENTED_EDGE ( 'NONE', *, *, #2613, .F. ) ;
#2951 = AXIS2_PLACEMENT_3D ( 'NONE', #883, #2587, #1068 ) ;
#2952 = ORIENTED_EDGE ( 'NONE', *, *, #2800, .F. ) ;
#2953 = PLANE ( 'NONE',  #2347 ) ;
#2954 = PRODUCT ( 'MAS-165', 'MAS-165', '', ( #3221 ) ) ;
#2955 = CARTESIAN_POINT ( 'NONE',  ( 1.040000000000000036, -0.8660254037844384856, -0.5000000000000003331 ) ) ;
#2956 = DIRECTION ( 'NONE',  ( 0.000000000000000000, 0.000000000000000000, -1.000000000000000000 ) ) ;
#2957 = CARTESIAN_POINT ( 'NONE',  ( 38.49999999999999289, 1.474514954580286030E-14, 16.49999999999999289 ) ) ;
#2958 = DIRECTION ( 'NONE',  ( 1.000000000000000000, -0.000000000000000000, -0.000000000000000000 ) ) ;
#2959 = ADVANCED_FACE ( 'NONE', ( #383 ), #2127, .T. ) ;
#2960 = CYLINDRICAL_SURFACE ( 'NONE', #1000, 5.000000000000000888 ) ;
#2961 = CARTESIAN_POINT ( 'NONE',  ( 100.0000000000000000, -6.928842772166554697E-15, 7.500000000000000000 ) ) ;
#2962 = CARTESIAN_POINT ( 'NONE',  ( 87.00000000000000000, -7.010408762983600216E-15, 2.499999999999999556 ) ) ;
#2963 = ORIENTED_EDGE ( 'NONE', *, *, #839, .T. ) ;
#2964 = EDGE_CURVE ( 'NONE', #628, #914, #2113, .T. ) ;
#2965 = VERTEX_POINT ( 'NONE', #846 ) ;
#2966 = COLOUR_RGB ( '',0.8941176470588234615, 0.8941176470588234615, 0.8941176470588234615 ) ;
#2967 = LINE ( 'NONE', #728, #1586 ) ;
#2968 = CARTESIAN_POINT ( 'NONE',  ( -41.99999999999999289, -6.449497959004950529E-15, 15.00000000000000000 ) ) ;
#2969 = FACE_BOUND ( 'NONE', #478, .T. ) ;
#2970 = EDGE_CURVE ( 'NONE', #2427, #91, #1111, .T. ) ;
#2971 = DIRECTION ( 'NONE',  ( 1.000000000000000000, 0.000000000000000000, 0.000000000000000000 ) ) ;
#2972 = FILL_AREA_STYLE ('',( #1311 ) ) ;
#2973 = VECTOR ( 'NONE', #2693, 1000.000000000000000 ) ;
#2974 = VERTEX_POINT ( 'NONE', #627 ) ;
#2975 = DIRECTION ( 'NONE',  ( 0.000000000000000000, 0.000000000000000000, 1.000000000000000000 ) ) ;
#2976 = EDGE_CURVE ( 'NONE', #2118, #2088, #832, .T. ) ;
#2977 = PRODUCT_DEFINITION_SHAPE ( 'NONE', 'NONE',  #2854 ) ;
#2978 = CARTESIAN_POINT ( 'NONE',  ( 100.0000000000000000, -6.928842772166554697E-15, 12.50000000000000000 ) ) ;
#2979 = AXIS2_PLACEMENT_3D ( 'NONE', #1858, #2137, #98 ) ;
#2980 = ORIENTED_EDGE ( 'NONE', *, *, #2193, .T. ) ;
#2981 = ORIENTED_EDGE ( 'NONE', *, *, #2262, .T. ) ;
#2982 = CIRCLE ( 'NONE', #1697, 5.000000000000000888 ) ;
#2983 = CIRCLE ( 'NONE', #904, 13.00000000000000178 ) ;
#2984 = CIRCLE ( 'NONE', #496, 1.499999999999999778 ) ;
#2985 = LINE ( 'NONE', #1013, #3196 ) ;
#2986 = CARTESIAN_POINT ( 'NONE',  ( 1.040000000000000036, 1.154700538379252350, -1.084202172485497162E-16 ) ) ;
#2987 = DIRECTION ( 'NONE',  ( 1.000000000000000000, 2.312964634635742957E-16, 0.000000000000000000 ) ) ;
#2988 = DIRECTION ( 'NONE',  ( 0.000000000000000000, 0.000000000000000000, 1.000000000000000000 ) ) ;
#2989 =( GEOMETRIC_REPRESENTATION_CONTEXT ( 3 ) GLOBAL_UNCERTAINTY_ASSIGNED_CONTEXT ( ( #2658 ) ) GLOBAL_UNIT_ASSIGNED_CONTEXT ( ( #1959, #240, #506 ) ) REPRESENTATION_CONTEXT ( 'NONE', 'WORKASPACE' ) );
#2990 = CARTESIAN_POINT ( 'NONE',  ( 37.00000000000000000, 1.474514954580286030E-14, 20.99999999999999645 ) ) ;
#2991 =( NAMED_UNIT ( * ) SI_UNIT ( $, .STERADIAN. ) SOLID_ANGLE_UNIT ( ) );
#2992 = ORIENTED_EDGE ( 'NONE', *, *, #2593, .F. ) ;
#2993 = LINE ( 'NONE', #2071, #14 ) ;
#2994 =( LENGTH_UNIT ( ) NAMED_UNIT ( * ) SI_UNIT ( .MILLI., .METRE. ) );
#2995 = DIRECTION ( 'NONE',  ( -0.000000000000000000, -0.000000000000000000, -1.000000000000000000 ) ) ;
#2996 = DIRECTION ( 'NONE',  ( -1.000000000000000000, -2.312964634635742957E-16, 0.000000000000000000 ) ) ;
#2997 = EDGE_CURVE ( 'NONE', #861, #2776, #481, .T. ) ;
#2998 = VERTEX_POINT ( 'NONE', #335 ) ;
#2999 = ORIENTED_EDGE ( 'NONE', *, *, #184, .F. ) ;
#3000 = CARTESIAN_POINT ( 'NONE',  ( 27.00000000000000000, -7.622732162557277534E-15, 7.500000000000000000 ) ) ;
#3001 = VECTOR ( 'NONE', #631, 1000.000000000000000 ) ;
#3002 = CARTESIAN_POINT ( 'NONE',  ( 36.33339417452629050, -1.347339434735542074, 16.39865934157270644 ) ) ;
#3003 = CARTESIAN_POINT ( 'NONE',  ( 35.75000000000000000, 1.489823039569627924E-14, 12.99999999999999822 ) ) ;
#3004 = LINE ( 'NONE', #1777, #1105 ) ;
#3005 = AXIS2_PLACEMENT_3D ( 'NONE', #1241, #3217, #2468 ) ;
#3006 = DIRECTION ( 'NONE',  ( 0.000000000000000000, 0.000000000000000000, -1.000000000000000000 ) ) ;
#3007 =( LENGTH_UNIT ( ) NAMED_UNIT ( * ) SI_UNIT ( .MILLI., .METRE. ) );
#3008 = EDGE_LOOP ( 'NONE', ( #105, #421 ) ) ;
#3009 = CARTESIAN_POINT ( 'NONE',  ( 87.00000000000000000, -6.520550043324660412E-15, -1.499999999999992673 ) ) ;
#3010 = CYLINDRICAL_SURFACE ( 'NONE', #1640, 1.499999999999994449 ) ;
#3011 = CARTESIAN_POINT ( 'NONE',  ( -41.99999999999999289, -6.449497959004950529E-15, 15.00000000000000000 ) ) ;
#3012 = EDGE_LOOP ( 'NONE', ( #1585, #539, #558, #1371 ) ) ;
#3013 = ORIENTED_EDGE ( 'NONE', *, *, #1303, .T. ) ;
#3014 = EDGE_CURVE ( 'NONE', #488, #2839, #1955, .T. ) ;
#3015 = LINE ( 'NONE', #1087, #2616 ) ;
#3016 = CYLINDRICAL_SURFACE ( 'NONE', #739, 8.999999999999994671 ) ;
#3017 = CARTESIAN_POINT ( 'NONE',  ( -26.99999999999999645, -5.785761963836251101E-15, 2.500000000000000444 ) ) ;
#3018 = ORIENTED_EDGE ( 'NONE', *, *, #2906, .F. ) ;
#3019 = EDGE_CURVE ( 'NONE', #108, #359, #495, .T. ) ;
#3020 = CARTESIAN_POINT ( 'NONE',  ( -26.99999999999999645, -5.785761963836251101E-15, 7.500000000000000000 ) ) ;
#3021 = CARTESIAN_POINT ( 'NONE',  ( 140.0000000000000000, -6.928842772166554697E-15, 7.500000000000000000 ) ) ;
#3022 =( NAMED_UNIT ( * ) PLANE_ANGLE_UNIT ( ) SI_UNIT ( $, .RADIAN. ) );
#3023 = ORIENTED_EDGE ( 'NONE', *, *, #660, .T. ) ;
#3024 = ORIENTED_EDGE ( 'NONE', *, *, #2656, .T. ) ;
#3025 = AXIS2_PLACEMENT_3D ( 'NONE', #2433, #2910, #3169 ) ;
#3026 = CARTESIAN_POINT ( 'NONE',  ( 35.57671993710908964, 0.4836543419624541595, 16.48745487577124180 ) ) ;
#3027 =( NAMED_UNIT ( * ) SI_UNIT ( $, .STERADIAN. ) SOLID_ANGLE_UNIT ( ) );
#3028 = PLANE ( 'NONE',  #2197 ) ;
#3029 = APPLICATION_CONTEXT ( 'automotive_design' ) ;
#3030 = CARTESIAN_POINT ( 'NONE',  ( -41.99999999999999289, -1.109217911451089172E-14, 7.500000000000000000 ) ) ;
#3031 = VERTEX_POINT ( 'NONE', #2867 ) ;
#3032 = CIRCLE ( 'NONE', #1743, 41.99999999999999289 ) ;
#3033 = CARTESIAN_POINT ( 'NONE',  ( 38.25000000000000000, 1.474514954580286030E-14, 12.99999999999999822 ) ) ;
#3034 = CARTESIAN_POINT ( 'NONE',  ( 1.040000000000000036, 0.000000000000000000, 1.000000000000000000 ) ) ;
#3035 = FACE_BOUND ( 'NONE', #3008, .T. ) ;
#3036 = CLOSED_SHELL ( 'NONE', ( #1826, #2959, #1987, #414, #1263, #1776, #788, #360, #994, #1718, #1590, #2392, #2172, #296 ) ) ;
#3037 = EDGE_CURVE ( 'NONE', #1178, #2346, #2349, .T. ) ;
#3038 =( GEOMETRIC_REPRESENTATION_CONTEXT ( 3 ) GLOBAL_UNCERTAINTY_ASSIGNED_CONTEXT ( ( #1259 ) ) GLOBAL_UNIT_ASSIGNED_CONTEXT ( ( #2994, #1515, #2548 ) ) REPRESENTATION_CONTEXT ( 'NONE', 'WORKASPACE' ) );
#3039 = ORIENTED_EDGE ( 'NONE', *, *, #598, .T. ) ;
#3040 =( NAMED_UNIT ( * ) SI_UNIT ( $, .STERADIAN. ) SOLID_ANGLE_UNIT ( ) );
#3041 = CIRCLE ( 'NONE', #1641, 7.500000000000000000 ) ;
#3042 = ADVANCED_FACE ( 'NONE', ( #1831 ), #1622, .T. ) ;
#3043 = DIRECTION ( 'NONE',  ( -2.312964634635742957E-16, 1.000000000000000000, 0.000000000000000000 ) ) ;
#3044 = ORIENTED_EDGE ( 'NONE', *, *, #51, .T. ) ;
#3045 = ADVANCED_BREP_SHAPE_REPRESENTATION ( '', ( #3192, #2878 ), #1321 ) ;
#3046 = PRESENTATION_LAYER_ASSIGNMENT (  '', '', ( #1113 ) ) ;
#3047 =( GEOMETRIC_REPRESENTATION_CONTEXT ( 3 ) GLOBAL_UNCERTAINTY_ASSIGNED_CONTEXT ( ( #1920 ) ) GLOBAL_UNIT_ASSIGNED_CONTEXT ( ( #1479, #191, #458 ) ) REPRESENTATION_CONTEXT ( 'NONE', 'WORKASPACE' ) );
#3048 = EDGE_CURVE ( 'NONE', #359, #108, #2983, .T. ) ;
#3049 = DIRECTION ( 'NONE',  ( 0.000000000000000000, 0.000000000000000000, -1.000000000000000000 ) ) ;
#3050 = DIRECTION ( 'NONE',  ( -1.000000000000000000, -0.000000000000000000, -0.000000000000000000 ) ) ;
#3051 = DIRECTION ( 'NONE',  ( -1.000000000000000000, -2.312964634635742957E-16, 0.000000000000000000 ) ) ;
#3052 = ORIENTED_EDGE ( 'NONE', *, *, #1510, .T. ) ;
#3053 = DIRECTION ( 'NONE',  ( -2.478176394252581634E-16, 1.000000000000000000, 0.000000000000000000 ) ) ;
#3054 = CARTESIAN_POINT ( 'NONE',  ( 87.00000000000000000, -7.622732162557277534E-15, 7.500000000000000000 ) ) ;
#3055 = EDGE_LOOP ( 'NONE', ( #2255, #611, #2740, #2485, #669, #2134 ) ) ;
#3056 = LINE ( 'NONE', #2604, #844 ) ;
#3057 = LINE ( 'NONE', #2081, #3001 ) ;
#3058 = ORIENTED_EDGE ( 'NONE', *, *, #1490, .F. ) ;
#3059 = VECTOR ( 'NONE', #2560, 1000.000000000000000 ) ;
#3060 = EDGE_CURVE ( 'NONE', #1226, #546, #849, .T. ) ;
#3061 = CARTESIAN_POINT ( 'NONE',  ( 38.45202114561161011, 0.3888602178275711863, 16.49210820886665019 ) ) ;
#3062 = ORIENTED_EDGE ( 'NONE', *, *, #2147, .T. ) ;
#3063 = CARTESIAN_POINT ( 'NONE',  ( 27.00000000000000000, 6.704247063196759979E-15, 7.500000000000000000 ) ) ;
#3064 = DIRECTION ( 'NONE',  ( 0.000000000000000000, 0.000000000000000000, 1.000000000000000000 ) ) ;
#3065 = ORIENTED_EDGE ( 'NONE', *, *, #909, .T. ) ;
#3066 = DIRECTION ( 'NONE',  ( 0.000000000000000000, 0.000000000000000000, -1.000000000000000000 ) ) ;
#3067 = CARTESIAN_POINT ( 'NONE',  ( 100.0000000000000000, -5.336801933274995404E-15, -5.500000000000001776 ) ) ;
#3068 = AXIS2_PLACEMENT_3D ( 'NONE', #2873, #3102, #563 ) ;
#3069 = VERTEX_POINT ( 'NONE', #2319 ) ;
#3070 = CARTESIAN_POINT ( 'NONE',  ( 150.0000000000000000, -6.928842772166554697E-15, 7.500000000000000000 ) ) ;
#3071 = CARTESIAN_POINT ( 'NONE',  ( 0.000000000000000000, 0.000000000000000000, 0.000000000000000000 ) ) ;
#3072 = CONICAL_SURFACE ( 'NONE', #688, 1.219500000000000028, 0.7853981633974487231 ) ;
#3073 = ADVANCED_FACE ( 'NONE', ( #130 ), #3077, .T. ) ;
#3074 = EDGE_LOOP ( 'NONE', ( #1842, #2303, #1237, #129 ) ) ;
#3075 = ORIENTED_EDGE ( 'NONE', *, *, #2701, .F. ) ;
#3076 = CARTESIAN_POINT ( 'NONE',  ( -37.00000000000000000, -5.785761963836251101E-15, 7.500000000000000000 ) ) ;
#3077 = PLANE ( 'NONE',  #1270 ) ;
#3078 = ORIENTED_EDGE ( 'NONE', *, *, #799, .T. ) ;
#3079 = CIRCLE ( 'NONE', #1258, 1.499999999999994449 ) ;
#3080 = CARTESIAN_POINT ( 'NONE',  ( 60.00000000000000000, -6.928842772166554697E-15, 7.500000000000000000 ) ) ;
#3081 = AXIS2_PLACEMENT_3D ( 'NONE', #814, #281, #1583 ) ;
#3082 = FACE_OUTER_BOUND ( 'NONE', #3106, .T. ) ;
#3083 = ORIENTED_EDGE ( 'NONE', *, *, #1463, .F. ) ;
#3084 = CIRCLE ( 'NONE', #2932, 5.000000000000000000 ) ;
#3085 = VERTEX_POINT ( 'NONE', #402 ) ;
#3086 = CARTESIAN_POINT ( 'NONE',  ( 100.0000000000000000, -6.928842772166554697E-15, 7.500000000000000000 ) ) ;
#3087 = VECTOR ( 'NONE', #1266, 1000.000000000000000 ) ;
#3088 =( LENGTH_UNIT ( ) NAMED_UNIT ( * ) SI_UNIT ( .MILLI., .METRE. ) );
#3089 =( GEOMETRIC_REPRESENTATION_CONTEXT ( 3 ) GLOBAL_UNCERTAINTY_ASSIGNED_CONTEXT ( ( #777 ) ) GLOBAL_UNIT_ASSIGNED_CONTEXT ( ( #1533, #1082, #3027 ) ) REPRESENTATION_CONTEXT ( 'NONE', 'WORKASPACE' ) );
#3090 = PRODUCT_DEFINITION_FORMATION_WITH_SPECIFIED_SOURCE ( 'ANY', '', #2954, .NOT_KNOWN. ) ;
#3091 = CARTESIAN_POINT ( 'NONE',  ( 140.0000000000000000, -5.336801933274995404E-15, -5.500000000000001776 ) ) ;
#3092 = ORIENTED_EDGE ( 'NONE', *, *, #436, .F. ) ;
#3093 = EDGE_CURVE ( 'NONE', #1756, #815, #1168, .T. ) ;
#3094 = PRODUCT_DEFINITION ( 'UNKNOWN', '', #19, #1809 ) ;
#3095 = VERTEX_POINT ( 'NONE', #2641 ) ;
#3096 = DIRECTION ( 'NONE',  ( -1.000000000000000000, -0.000000000000000000, -0.000000000000000000 ) ) ;
#3097 = ORIENTED_EDGE ( 'NONE', *, *, #1067, .F. ) ;
#3098 = DIRECTION ( 'NONE',  ( 0.000000000000000000, 0.000000000000000000, -1.000000000000000000 ) ) ;
#3099 = DIRECTION ( 'NONE',  ( -1.000000000000000000, -0.000000000000000000, -0.000000000000000000 ) ) ;
#3100 = VERTEX_POINT ( 'NONE', #416 ) ;
#3101 = ORIENTED_EDGE ( 'NONE', *, *, #2440, .T. ) ;
#3102 = DIRECTION ( 'NONE',  ( 1.000000000000000000, -0.000000000000000000, -0.000000000000000000 ) ) ;
#3103 = LINE ( 'NONE', #2121, #439 ) ;
#3104 = VECTOR ( 'NONE', #2574, 1000.000000000000114 ) ;
#3105 = DIRECTION ( 'NONE',  ( -1.000000000000000000, 0.000000000000000000, 0.000000000000000000 ) ) ;
#3106 = EDGE_LOOP ( 'NONE', ( #1297, #2918, #2491, #752, #2289 ) ) ;
#3107 = UNCERTAINTY_MEASURE_WITH_UNIT (LENGTH_MEASURE( 1.000000000000000082E-05 ), #982, 'distance_accuracy_value', 'NONE');
#3108 = DIRECTION ( 'NONE',  ( -0.000000000000000000, 0.000000000000000000, -1.000000000000000000 ) ) ;
#3109 = ORIENTED_EDGE ( 'NONE', *, *, #436, .T. ) ;
#3110 = CARTESIAN_POINT ( 'NONE',  ( 150.0000000000000000, -6.316519372592878167E-15, 12.50000000000000000 ) ) ;
#3111 = ORIENTED_EDGE ( 'NONE', *, *, #273, .T. ) ;
#3112 = DIRECTION ( 'NONE',  ( -1.000000000000000000, -0.000000000000000000, -0.000000000000000000 ) ) ;
#3113 = DIRECTION ( 'NONE',  ( -2.478176394252581634E-16, 1.000000000000000000, 0.000000000000000000 ) ) ;
#3114 = ADVANCED_FACE ( 'NONE', ( #431 ), #2445, .T. ) ;
#3115 = DIRECTION ( 'NONE',  ( 0.000000000000000000, 0.000000000000000000, 1.000000000000000000 ) ) ;
#3116 = ORIENTED_EDGE ( 'NONE', *, *, #2033, .T. ) ;
#3117 = VERTEX_POINT ( 'NONE', #2673 ) ;
#3118 = CARTESIAN_POINT ( 'NONE',  ( 1.040000000000000036, 0.000000000000000000, 0.000000000000000000 ) ) ;
#3119 = PLANE ( 'NONE',  #2206 ) ;
#3120 = CIRCLE ( 'NONE', #1513, 2.849999999999999645 ) ;
#3121 = UNCERTAINTY_MEASURE_WITH_UNIT (LENGTH_MEASURE( 1.000000000000000082E-05 ), #1854, 'distance_accuracy_value', 'NONE');
#3122 = FILL_AREA_STYLE ('',( #1138 ) ) ;
#3123 = MECHANICAL_DESIGN_GEOMETRIC_PRESENTATION_REPRESENTATION (  '', ( #2250 ), #633 ) ;
#3124 = CARTESIAN_POINT ( 'NONE',  ( 0.000000000000000000, 0.5773502691896263972, -1.000000000000000000 ) ) ;
#3125 = ORIENTED_EDGE ( 'NONE', *, *, #1734, .F. ) ;
#3126 = LINE ( 'NONE', #2887, #869 ) ;
#3127 = AXIS2_PLACEMENT_3D ( 'NONE', #918, #2400, #217 ) ;
#3128 = VERTEX_POINT ( 'NONE', #2411 ) ;
#3129 = CARTESIAN_POINT ( 'NONE',  ( 36.58213974117524714, 0.1061604454658580249, 12.49999999999999822 ) ) ;
#3130 = VERTEX_POINT ( 'NONE', #212 ) ;
#3131 = DIRECTION ( 'NONE',  ( 0.000000000000000000, -1.000000000000000000, 0.000000000000000000 ) ) ;
#3132 = DIRECTION ( 'NONE',  ( -1.000000000000000000, -0.000000000000000000, -0.000000000000000000 ) ) ;
#3133 = SHAPE_DEFINITION_REPRESENTATION ( #8, #524 ) ;
#3134 = ORIENTED_EDGE ( 'NONE', *, *, #1508, .T. ) ;
#3135 = VECTOR ( 'NONE', #1927, 1000.000000000000114 ) ;
#3136 = EDGE_CURVE ( 'NONE', #2825, #1108, #550, .T. ) ;
#3137 = CARTESIAN_POINT ( 'NONE',  ( 0.000000000000000000, 1.154700538379252350, -1.084202172485497162E-16 ) ) ;
#3138 =( LENGTH_UNIT ( ) NAMED_UNIT ( * ) SI_UNIT ( .MILLI., .METRE. ) );
#3139 = CLOSED_SHELL ( 'NONE', ( #2816, #2104, #2528, #3114, #1022, #29, #862, #2230, #1174, #3177, #1960, #2732, #1034, #2232, #2575, #2662, #2802, #176, #100, #2900, #2270, #123, #24, #1845, #1663, #1564, #1345 ) ) ;
#3140 = AXIS2_PLACEMENT_3D ( 'NONE', #2321, #1066, #322 ) ;
#3141 = VECTOR ( 'NONE', #1254, 1000.000000000000000 ) ;
#3142 = DIRECTION ( 'NONE',  ( 1.000000000000000000, 2.312964634635742957E-16, 0.000000000000000000 ) ) ;
#3143 = ORIENTED_EDGE ( 'NONE', *, *, #1092, .F. ) ;
#3144 = CARTESIAN_POINT ( 'NONE',  ( -23.99999999999999645, -6.928842772166554697E-15, 7.500000000000000000 ) ) ;
#3145 = AXIS2_PLACEMENT_3D ( 'NONE', #1355, #1870, #1376 ) ;
#3146 = EDGE_LOOP ( 'NONE', ( #382, #3134, #1662, #1033 ) ) ;
#3147 = CARTESIAN_POINT ( 'NONE',  ( 47.00000000000000000, 1.243235845170086321E-14, 16.49999999999999289 ) ) ;
#3148 = EDGE_LOOP ( 'NONE', ( #1811, #2476, #1901, #2195 ) ) ;
#3149 = CARTESIAN_POINT ( 'NONE',  ( 100.0000000000000000, -6.928842772166554697E-15, 19.50000000000000000 ) ) ;
#3150 = PLANE ( 'NONE',  #1784 ) ;
#3151 = LINE ( 'NONE', #902, #2637 ) ;
#3152 =( NAMED_UNIT ( * ) SI_UNIT ( $, .STERADIAN. ) SOLID_ANGLE_UNIT ( ) );
#3153 = ORIENTED_EDGE ( 'NONE', *, *, #1892, .T. ) ;
#3154 = FACE_OUTER_BOUND ( 'NONE', #1871, .T. ) ;
#3155 = LINE ( 'NONE', #924, #746 ) ;
#3156 = SURFACE_STYLE_FILL_AREA ( #2648 ) ;
#3157 = ADVANCED_FACE ( 'NONE', ( #2269 ), #198, .F. ) ;
#3158 = AXIS2_PLACEMENT_3D ( 'NONE', #3021, #1794, #1526 ) ;
#3159 = CARTESIAN_POINT ( 'NONE',  ( 1.040000000000000036, 0.5773502691896263972, 1.000000000000000000 ) ) ;
#3160 = ORIENTED_EDGE ( 'NONE', *, *, #947, .F. ) ;
#3161 = VECTOR ( 'NONE', #2621, 1000.000000000000000 ) ;
#3162 = FACE_OUTER_BOUND ( 'NONE', #3074, .T. ) ;
#3163 = ORIENTED_EDGE ( 'NONE', *, *, #1385, .T. ) ;
#3164 =( NAMED_UNIT ( * ) SI_UNIT ( $, .STERADIAN. ) SOLID_ANGLE_UNIT ( ) );
#3165 = ORIENTED_EDGE ( 'NONE', *, *, #2191, .T. ) ;
#3166 = EDGE_CURVE ( 'NONE', #1489, #585, #1401, .T. ) ;
#3167 = DIRECTION ( 'NONE',  ( -1.000000000000000000, -0.000000000000000000, -0.000000000000000000 ) ) ;
#3168 = B_SPLINE_CURVE_WITH_KNOTS ( 'NONE', 3,
 ( #1015, #787, #742, #237, #1230, #1981, #1493, #267, #2746, #2245 ),
 .UNSPECIFIED., .F., .F.,
 ( 4, 2, 2, 2, 4 ),
 ( 0.001487560081304217232, 0.001805301772647892973, 0.002123043463991568930, 0.002440785155335244670, 0.002758526846678920411 ),
 .UNSPECIFIED. ) ;
#3169 = DIRECTION ( 'NONE',  ( -2.478176394252581634E-16, 1.000000000000000000, 0.000000000000000000 ) ) ;
#3170 = DIRECTION ( 'NONE',  ( -1.000000000000000000, -0.000000000000000000, -0.000000000000000000 ) ) ;
#3171 = FILL_AREA_STYLE ('',( #2186 ) ) ;
#3172 = DIRECTION ( 'NONE',  ( -1.000000000000000000, -0.000000000000000000, -0.000000000000000000 ) ) ;
#3173 = DIRECTION ( 'NONE',  ( 0.000000000000000000, -1.000000000000000000, 0.000000000000000000 ) ) ;
#3174 = VECTOR ( 'NONE', #707, 1000.000000000000227 ) ;
#3175 = CARTESIAN_POINT ( 'NONE',  ( 38.30993956269966105, 0.7564481093111570242, 16.46997477067510118 ) ) ;
#3176 = APPLICATION_CONTEXT ( 'automotive_design' ) ;
#3177 = ADVANCED_FACE ( 'NONE', ( #1159, #1710 ), #679, .F. ) ;
#3178 = MANIFOLD_SOLID_BREP ( 'Boss-Extrude1', #3036 ) ;
#3179 = ORIENTED_EDGE ( 'NONE', *, *, #1797, .F. ) ;
#3180 = DIRECTION ( 'NONE',  ( 0.000000000000000000, 0.000000000000000000, 1.000000000000000000 ) ) ;
#3181 = ORIENTED_EDGE ( 'NONE', *, *, #2188, .F. ) ;
#3182 = EDGE_CURVE ( 'NONE', #2430, #1128, #1436, .T. ) ;
#3183 = DIRECTION ( 'NONE',  ( -1.000000000000000000, -0.000000000000000000, -0.000000000000000000 ) ) ;
#3184 = VECTOR ( 'NONE', #469, 1000.000000000000000 ) ;
#3185 = CYLINDRICAL_SURFACE ( 'NONE', #3127, 4.999999999999999112 ) ;
#3186 = CARTESIAN_POINT ( 'NONE',  ( 3.033375984251970081, -8.673617379884035472E-16, 0.000000000000000000 ) ) ;
#3187 = SHAPE_DEFINITION_REPRESENTATION ( #3214, #1790 ) ;
#3188 = SURFACE_SIDE_STYLE ('',( #1441 ) ) ;
#3189 = LINE ( 'NONE', #1173, #10 ) ;
#3190 = SURFACE_STYLE_FILL_AREA ( #1217 ) ;
#3191 = VECTOR ( 'NONE', #955, 1000.000000000000000 ) ;
#3192 = MANIFOLD_SOLID_BREP ( 'Boss-Extrude1', #2877 ) ;
#3193 = DIRECTION ( 'NONE',  ( -1.000000000000000000, -2.312964634635742957E-16, -0.000000000000000000 ) ) ;
#3194 = DIRECTION ( 'NONE',  ( 2.312964634635742957E-16, -1.000000000000000000, 0.000000000000000000 ) ) ;
#3195 = ORIENTED_EDGE ( 'NONE', *, *, #397, .T. ) ;
#3196 = VECTOR ( 'NONE', #3215, 1000.000000000000114 ) ;
#3197 = VERTEX_POINT ( 'NONE', #562 ) ;
#3198 = ADVANCED_FACE ( 'NONE', ( #1052 ), #450, .F. ) ;
#3199 = APPLICATION_CONTEXT ( 'automotive_design' ) ;
#3200 =( GEOMETRIC_REPRESENTATION_CONTEXT ( 3 ) GLOBAL_UNCERTAINTY_ASSIGNED_CONTEXT ( ( #3121 ) ) GLOBAL_UNIT_ASSIGNED_CONTEXT ( ( #1854, #1651, #3152 ) ) REPRESENTATION_CONTEXT ( 'NONE', 'WORKASPACE' ) );
#3201 = CARTESIAN_POINT ( 'NONE',  ( 0.000000000000000000, -0.5773502691896253980, 1.000000000000000000 ) ) ;
#3202 = CARTESIAN_POINT ( 'NONE',  ( 38.49023808469348040, -0.1968962347057416351, 16.49835841594091690 ) ) ;
#3203 = DIRECTION ( 'NONE',  ( -1.000000000000000000, 0.000000000000000000, 0.000000000000000000 ) ) ;
#3204 = CARTESIAN_POINT ( 'NONE',  ( 27.00000000000000000, 6.704247063196759979E-15, 7.500000000000000000 ) ) ;
#3205 = CARTESIAN_POINT ( 'NONE',  ( 1.750000000000000000, 0.000000000000000000, 0.000000000000000000 ) ) ;
#3206 = FACE_OUTER_BOUND ( 'NONE', #2538, .T. ) ;
#3207 = PRESENTATION_STYLE_ASSIGNMENT (( #2222 ) ) ;
#3208 = EDGE_CURVE ( 'NONE', #3100, #1030, #838, .T. ) ;
#3209 = CARTESIAN_POINT ( 'NONE',  ( 70.00000000000032685, -5.459266613189731341E-15, -4.500000000000000888 ) ) ;
#3210 = DIRECTION ( 'NONE',  ( -0.000000000000000000, 1.000000000000000000, -0.000000000000000000 ) ) ;
#3211 = ADVANCED_FACE ( 'NONE', ( #2284 ), #3010, .F. ) ;
#3212 = ORIENTED_EDGE ( 'NONE', *, *, #735, .F. ) ;
#3213 = VERTEX_POINT ( 'NONE', #2057 ) ;
#3214 = PRODUCT_DEFINITION_SHAPE ( 'NONE', 'NONE',  #2324 ) ;
#3215 = DIRECTION ( 'NONE',  ( -0.5000000000000042188, 1.060575238724903710E-16, -0.8660254037844361541 ) ) ;
#3216 = DIRECTION ( 'NONE',  ( -2.312964634635742957E-16, 1.000000000000000000, 0.000000000000000000 ) ) ;
#3217 = DIRECTION ( 'NONE',  ( 1.000000000000000000, 0.000000000000000000, -0.000000000000000000 ) ) ;
#3218 = CARTESIAN_POINT ( 'NONE',  ( 1.040000000000000036, -1.154700538379251684, 0.000000000000000000 ) ) ;
#3219 = ADVANCED_FACE ( 'NONE', ( #2328 ), #346, .T. ) ;
#3220 = DIRECTION ( 'NONE',  ( -1.000000000000000000, -0.000000000000000000, -0.000000000000000000 ) ) ;
#3221 = PRODUCT_CONTEXT ( 'NONE', #1516, 'mechanical' ) ;
#3222 = CARTESIAN_POINT ( 'NONE',  ( 27.00000000000000000, -7.622732162557277534E-15, 7.500000000000000000 ) ) ;
#3223 = NEXT_ASSEMBLY_USAGE_OCCURRENCE ( 'NAUO1', ' ', ' ', #1659, #254, $ ) ;
#3224 = NEXT_ASSEMBLY_USAGE_OCCURRENCE ( 'NAUO2', ' ', ' ', #1659, #694, $ ) ;
#3225 = NEXT_ASSEMBLY_USAGE_OCCURRENCE ( 'NAUO3', ' ', ' ', #1659, #3094, $ ) ;
#3226 = NEXT_ASSEMBLY_USAGE_OCCURRENCE ( 'NAUO4', ' ', ' ', #1659, #2324, $ ) ;
#3227 = NEXT_ASSEMBLY_USAGE_OCCURRENCE ( 'NAUO5', ' ', ' ', #1659, #2854, $ ) ;
#3228 = NEXT_ASSEMBLY_USAGE_OCCURRENCE ( 'NAUO6', ' ', ' ', #1659, #1264, $ ) ;
#3229 = NEXT_ASSEMBLY_USAGE_OCCURRENCE ( 'NAUO7', ' ', ' ', #1659, #499, $ ) ;
#3230=COLOUR_RGB('Dark Blue',0.08,0.2,0.34);
#3231=FILL_AREA_STYLE_COLOUR('',#3230);
#3232=FILL_AREA_STYLE('',(#3231));
#3233=SURFACE_STYLE_FILL_AREA(#3232);
#3234=SURFACE_SIDE_STYLE('',(#3233));
#3235=SURFACE_STYLE_USAGE(.BOTH.,#3234);
#3236=PRESENTATION_STYLE_ASSIGNMENT((#3235));
#3237=COLOUR_RGB('Light Blue',0.38,0.62,0.78);
#3238=FILL_AREA_STYLE_COLOUR('',#3237);
#3239=FILL_AREA_STYLE('',(#3238));
#3240=SURFACE_STYLE_FILL_AREA(#3239);
#3241=SURFACE_SIDE_STYLE('',(#3240));
#3242=SURFACE_STYLE_USAGE(.BOTH.,#3241);
#3243=PRESENTATION_STYLE_ASSIGNMENT((#3242));
#3244=COLOUR_RGB('Sky Blue',0.24,0.69,0.87);
#3245=FILL_AREA_STYLE_COLOUR('',#3244);
#3246=FILL_AREA_STYLE('',(#3245));
#3247=SURFACE_STYLE_FILL_AREA(#3246);
#3248=SURFACE_SIDE_STYLE('',(#3247));
#3249=SURFACE_STYLE_USAGE(.BOTH.,#3248);
#3250=PRESENTATION_STYLE_ASSIGNMENT((#3249));
#3251=COLOUR_RGB('Grey',0.48,0.52,0.57);
#3252=FILL_AREA_STYLE_COLOUR('',#3251);
#3253=FILL_AREA_STYLE('',(#3252));
#3254=SURFACE_STYLE_FILL_AREA(#3253);
#3255=SURFACE_SIDE_STYLE('',(#3254));
#3256=SURFACE_STYLE_USAGE(.BOTH.,#3255);
#3257=PRESENTATION_STYLE_ASSIGNMENT((#3256));
#3258=COLOUR_RGB('Black',0.12,0.14,0.17);
#3259=FILL_AREA_STYLE_COLOUR('',#3258);
#3260=FILL_AREA_STYLE('',(#3259));
#3261=SURFACE_STYLE_FILL_AREA(#3260);
#3262=SURFACE_SIDE_STYLE('',(#3261));
#3263=SURFACE_STYLE_USAGE(.BOTH.,#3262);
#3264=PRESENTATION_STYLE_ASSIGNMENT((#3263));
#3265=COLOUR_RGB('Off White',0.89,0.88,0.83);
#3266=FILL_AREA_STYLE_COLOUR('',#3265);
#3267=FILL_AREA_STYLE('',(#3266));
#3268=SURFACE_STYLE_FILL_AREA(#3267);
#3269=SURFACE_SIDE_STYLE('',(#3268));
#3270=SURFACE_STYLE_USAGE(.BOTH.,#3269);
#3271=PRESENTATION_STYLE_ASSIGNMENT((#3270));
ENDSEC;
END-ISO-10303-21;
